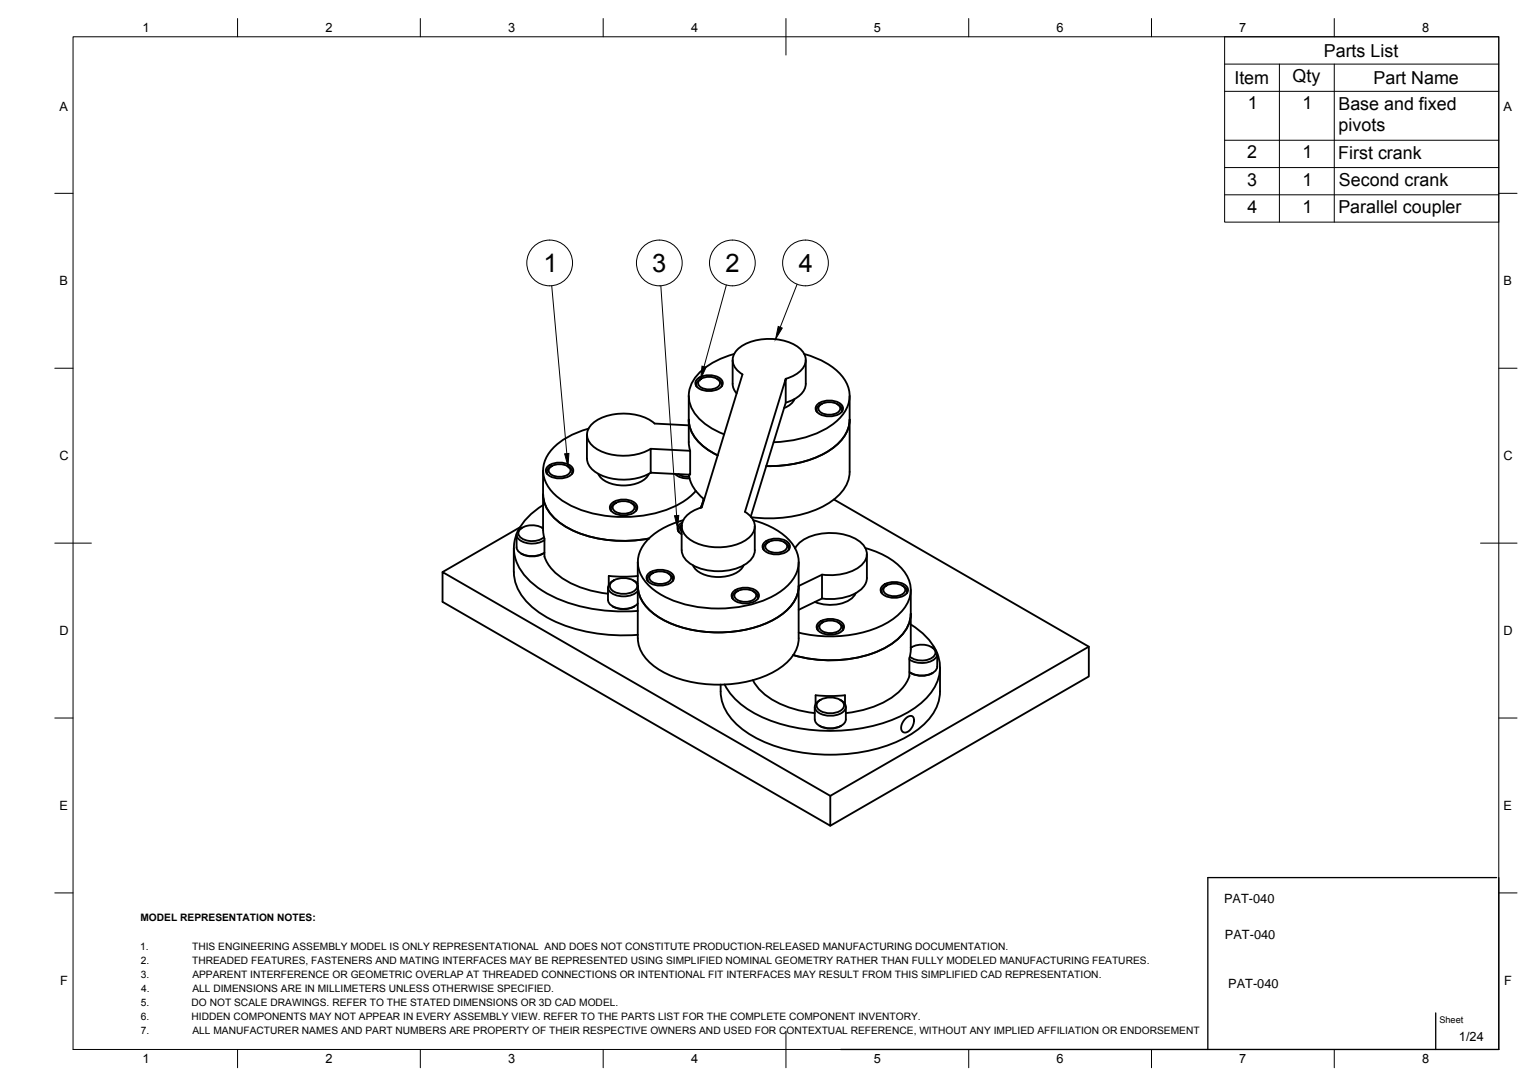
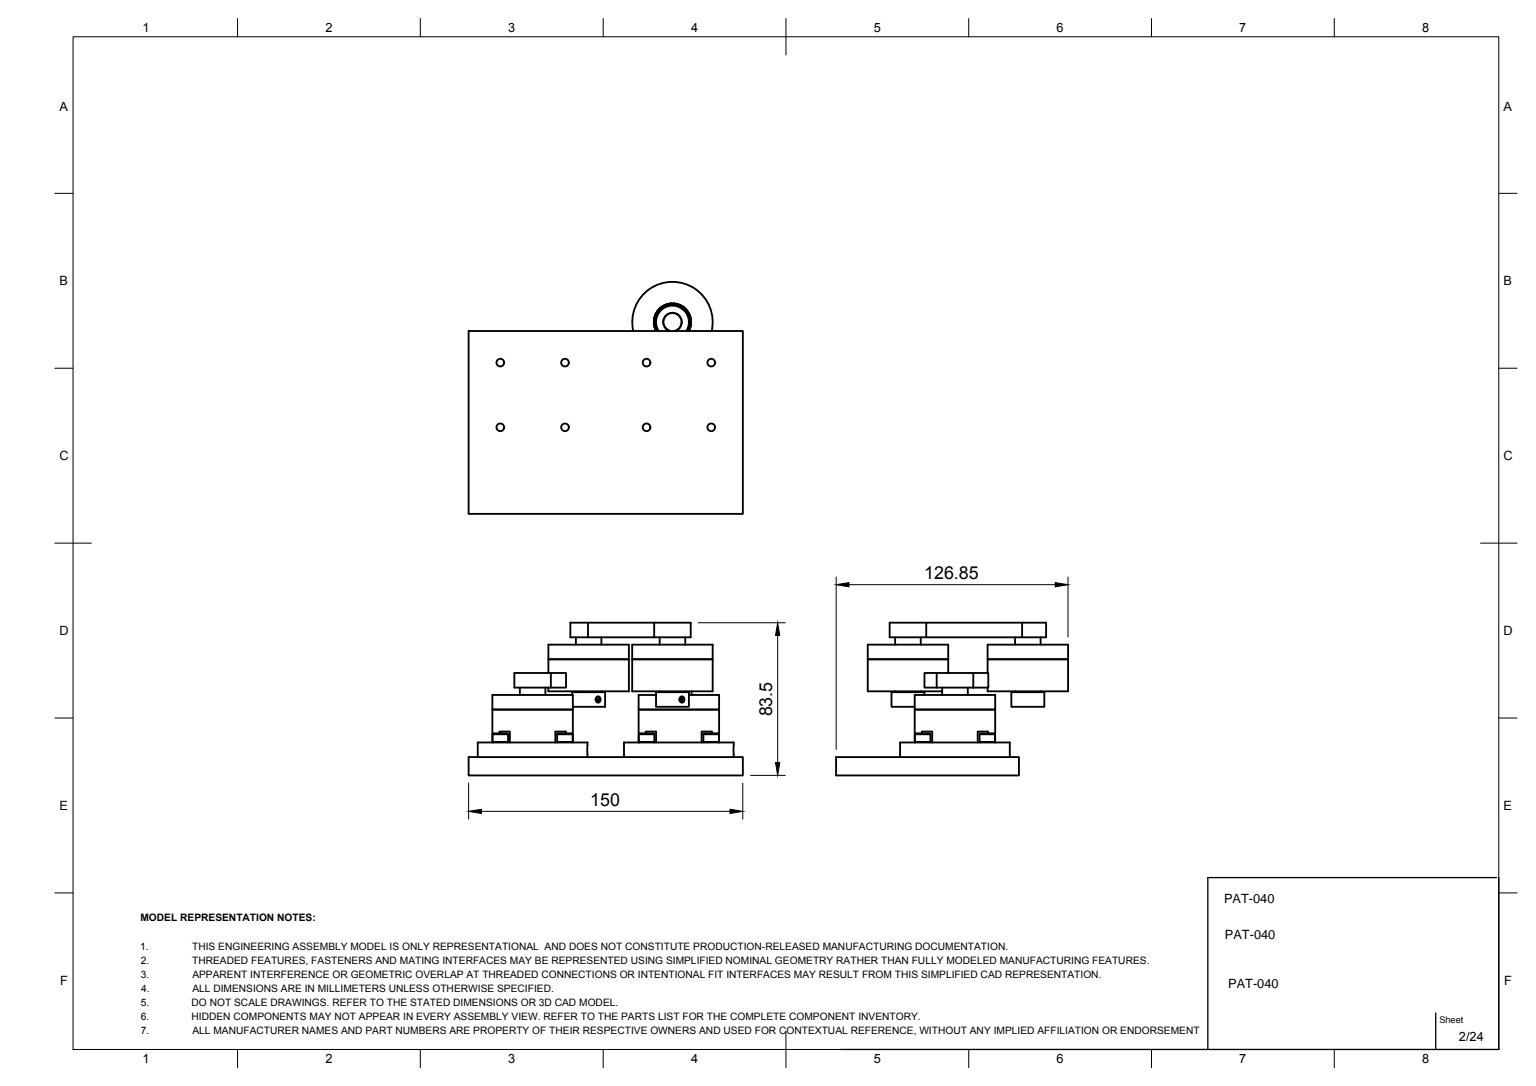
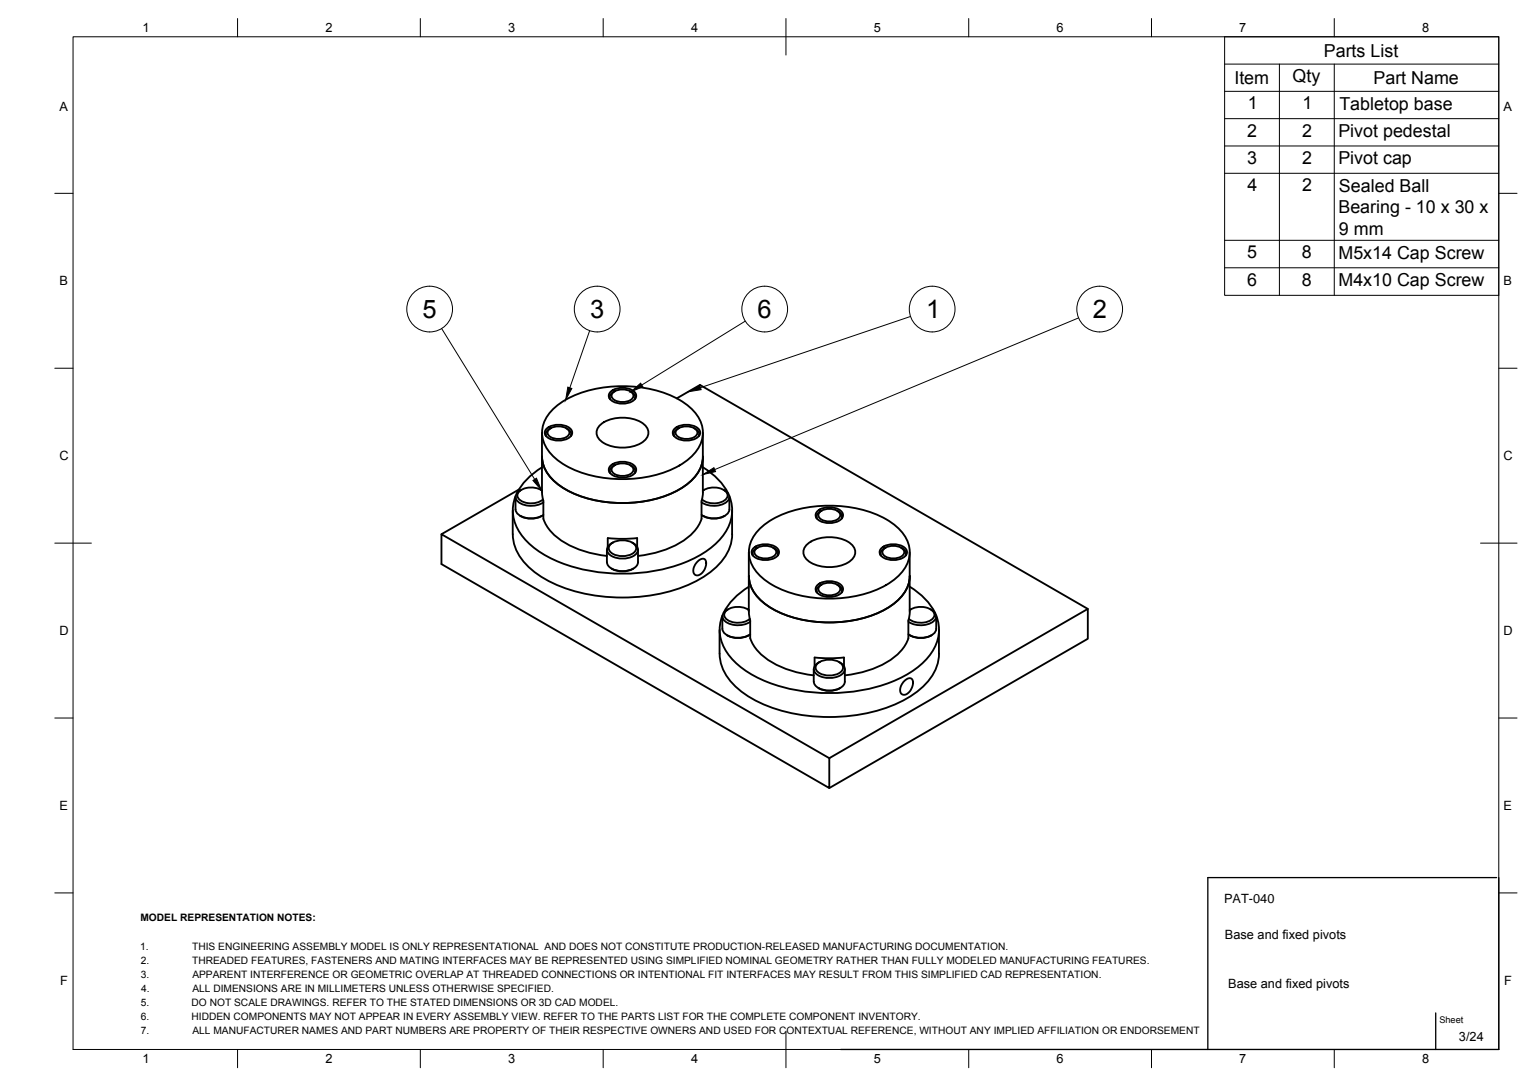
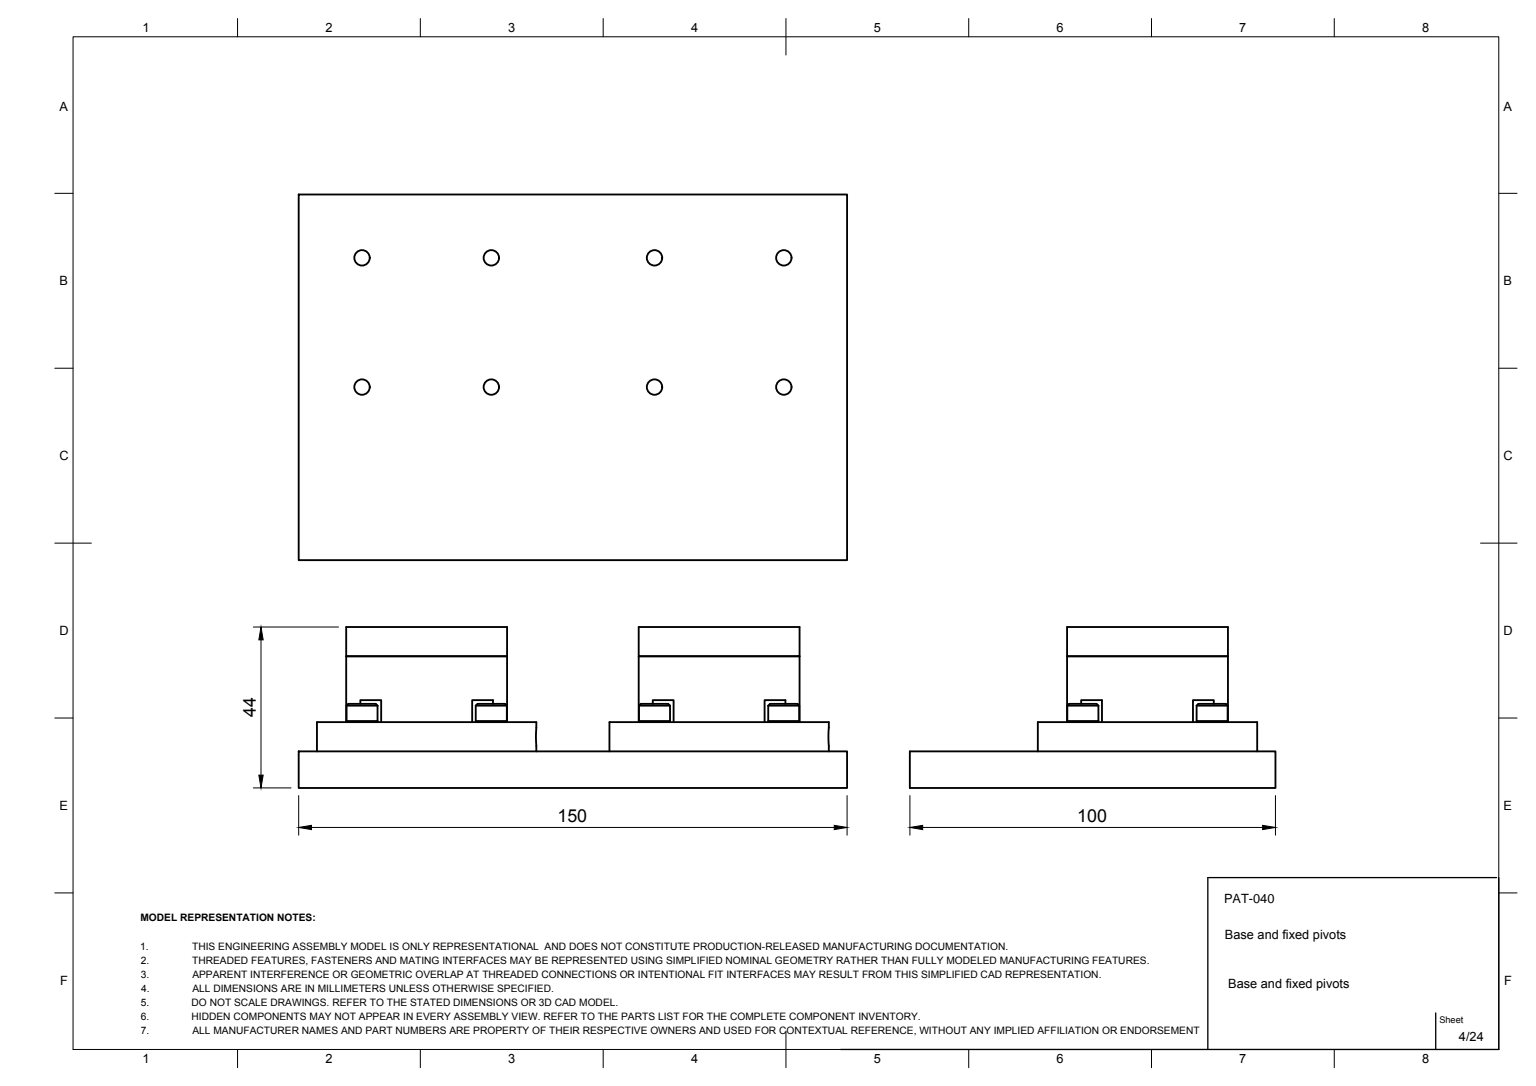
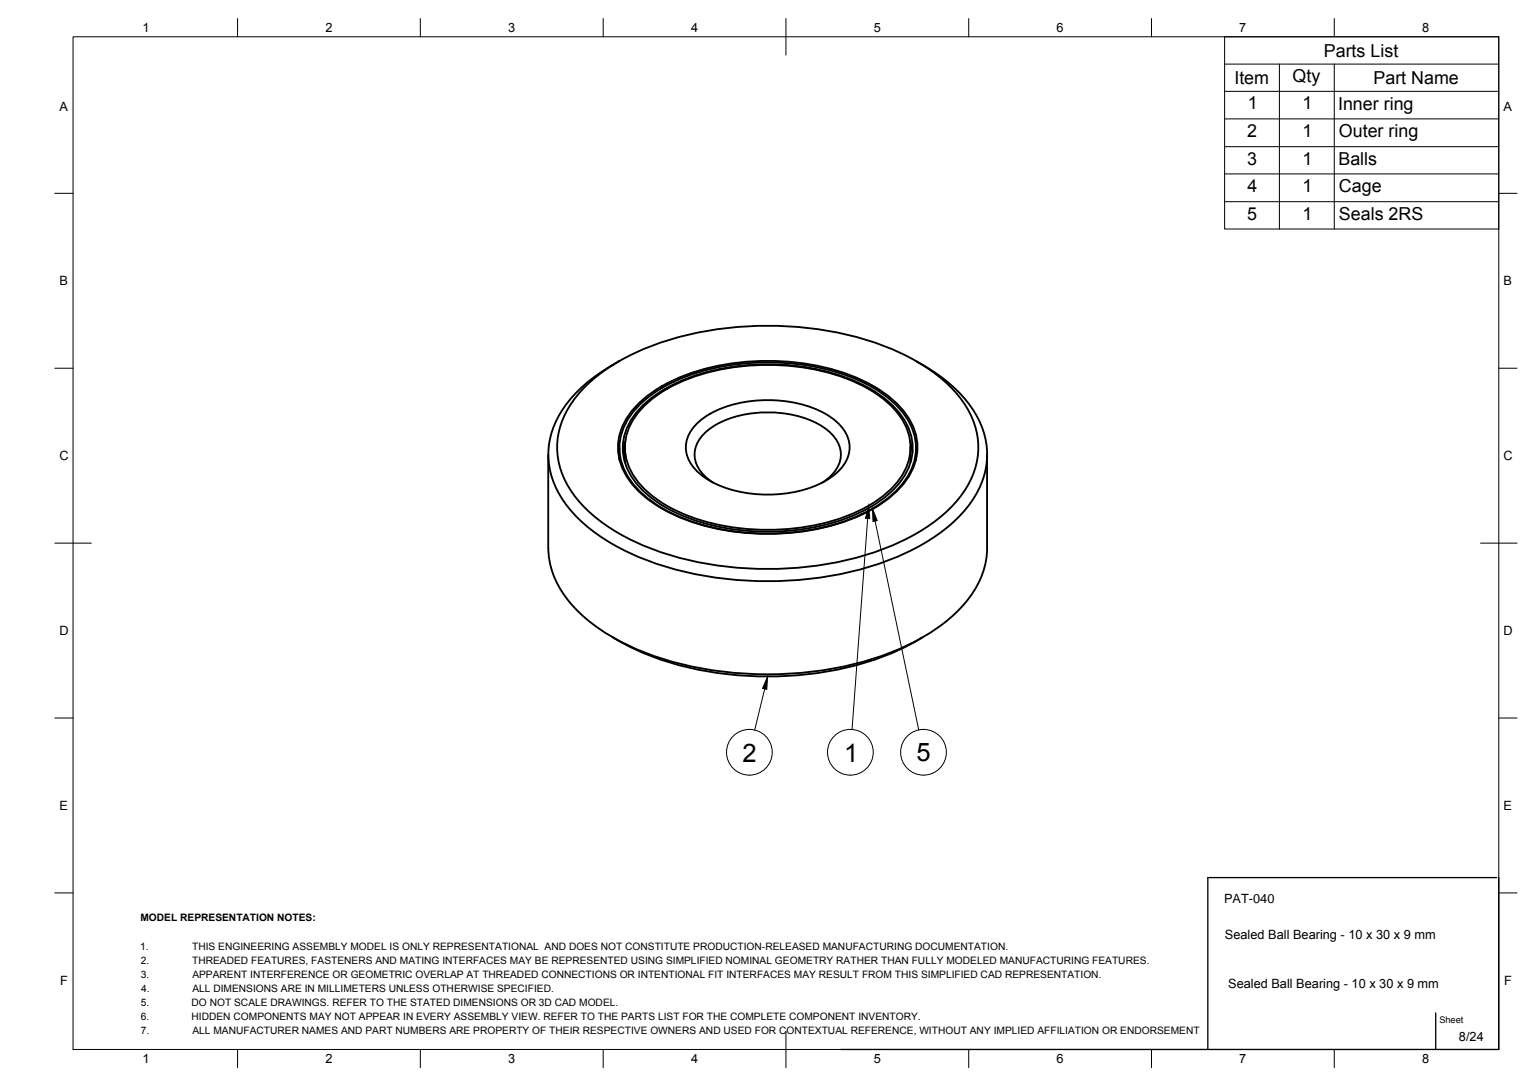
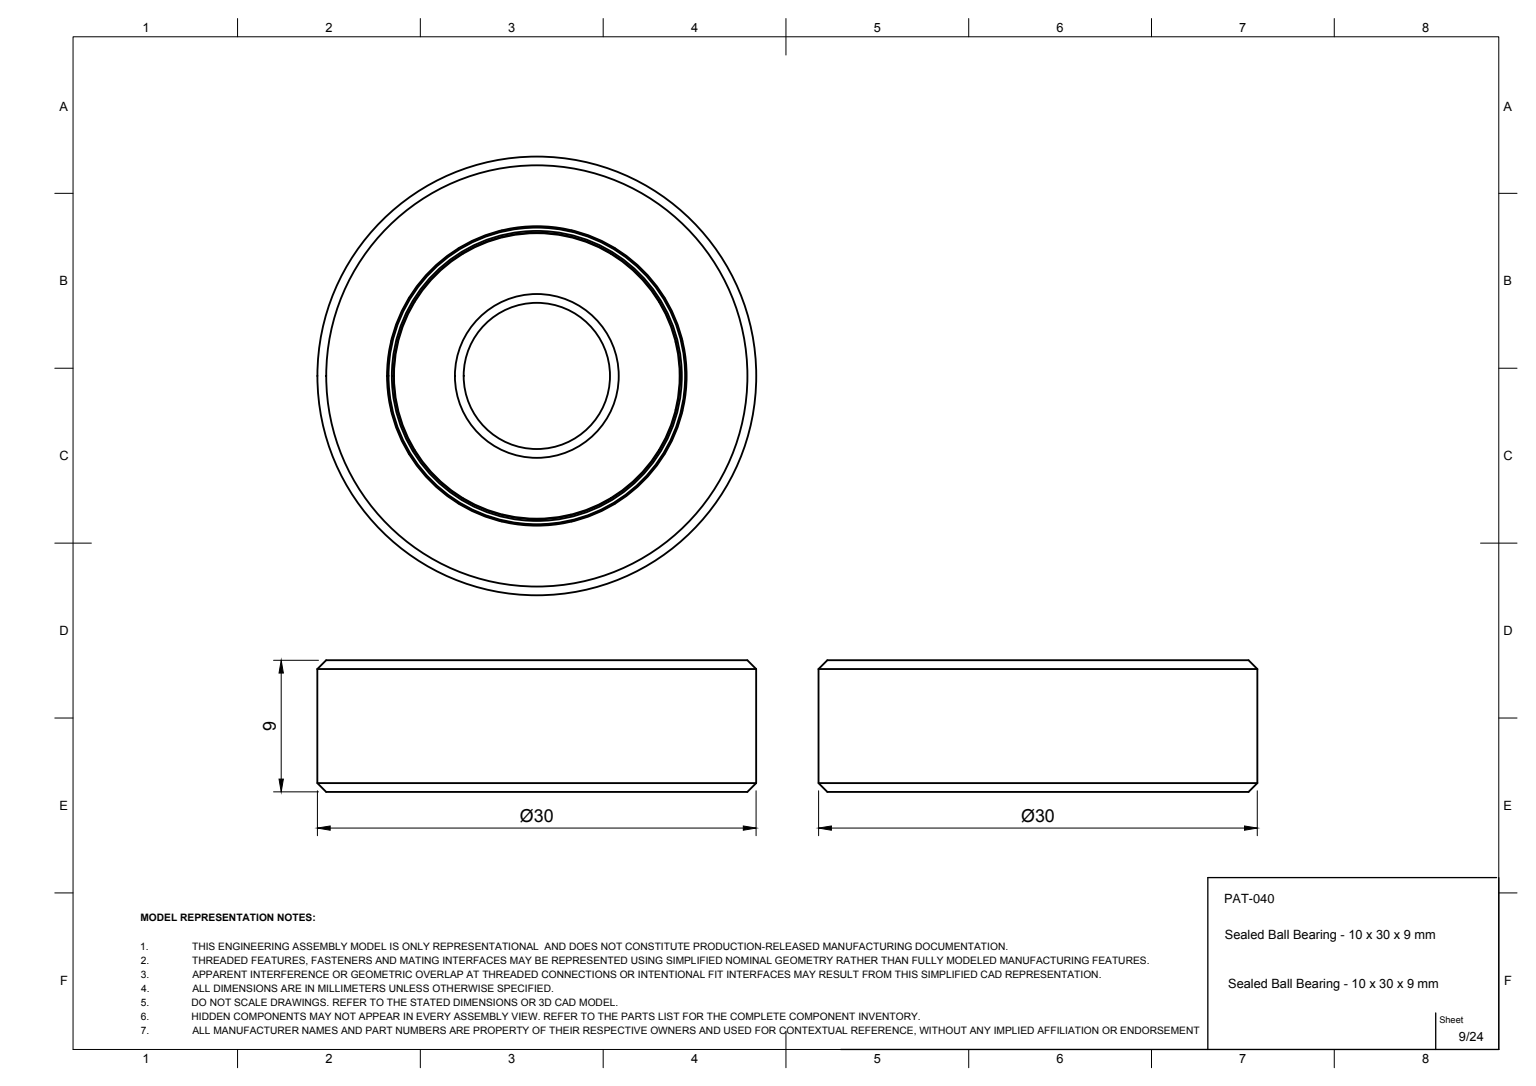
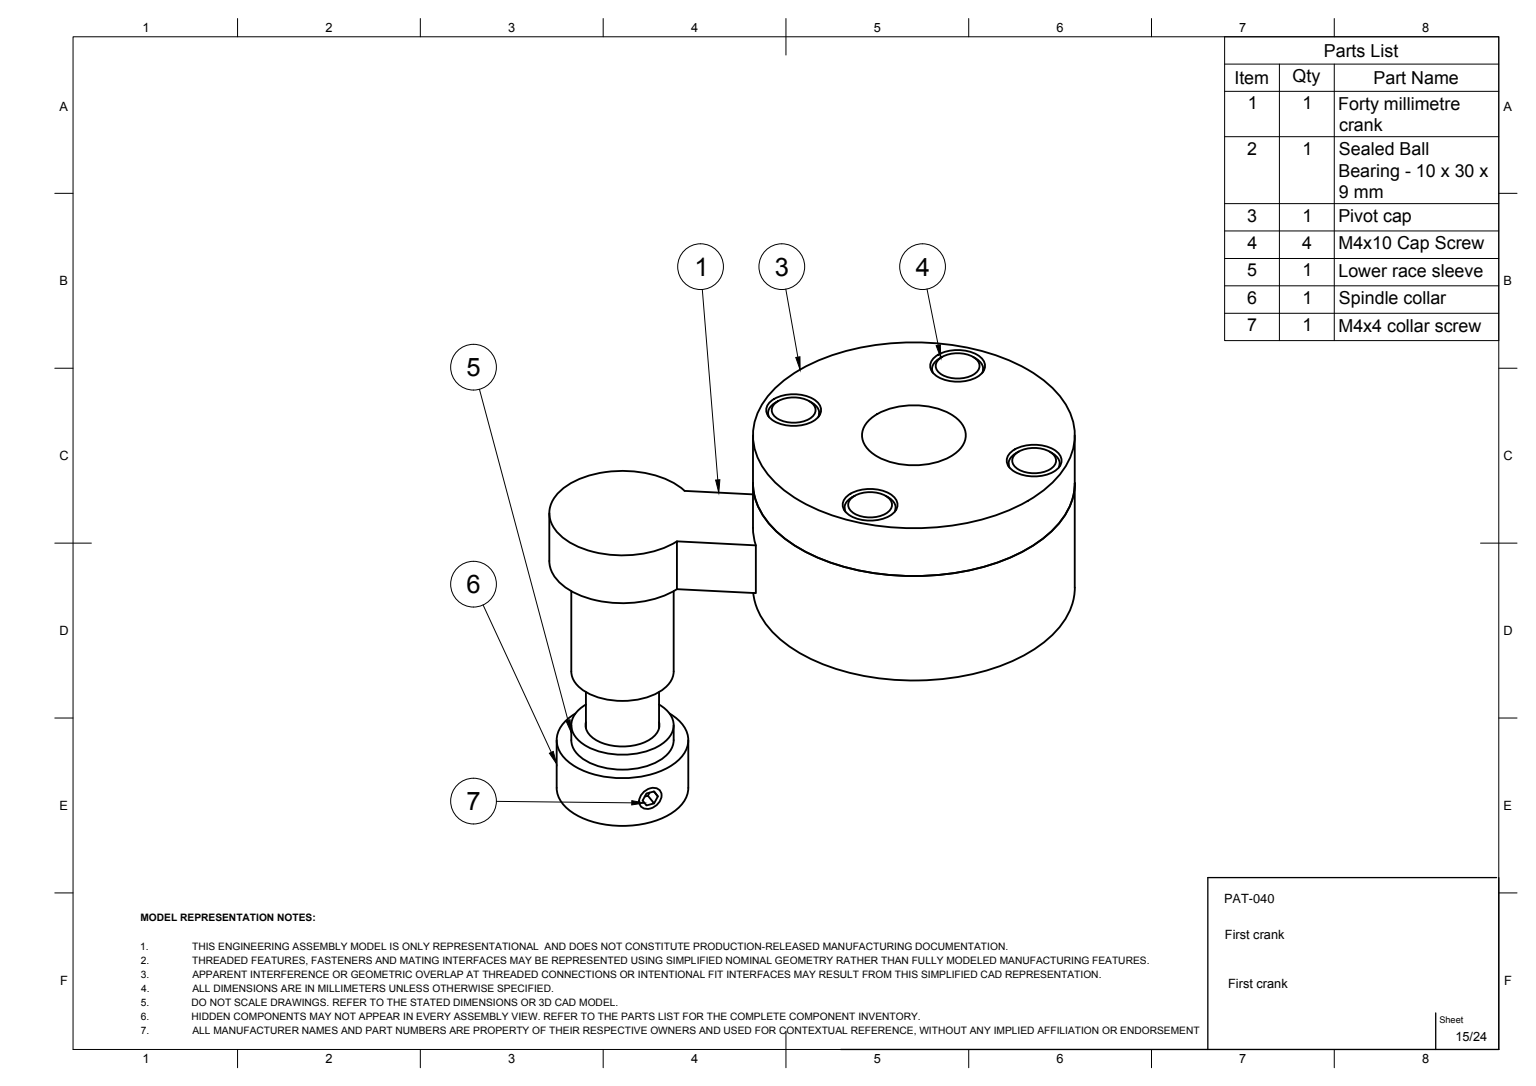
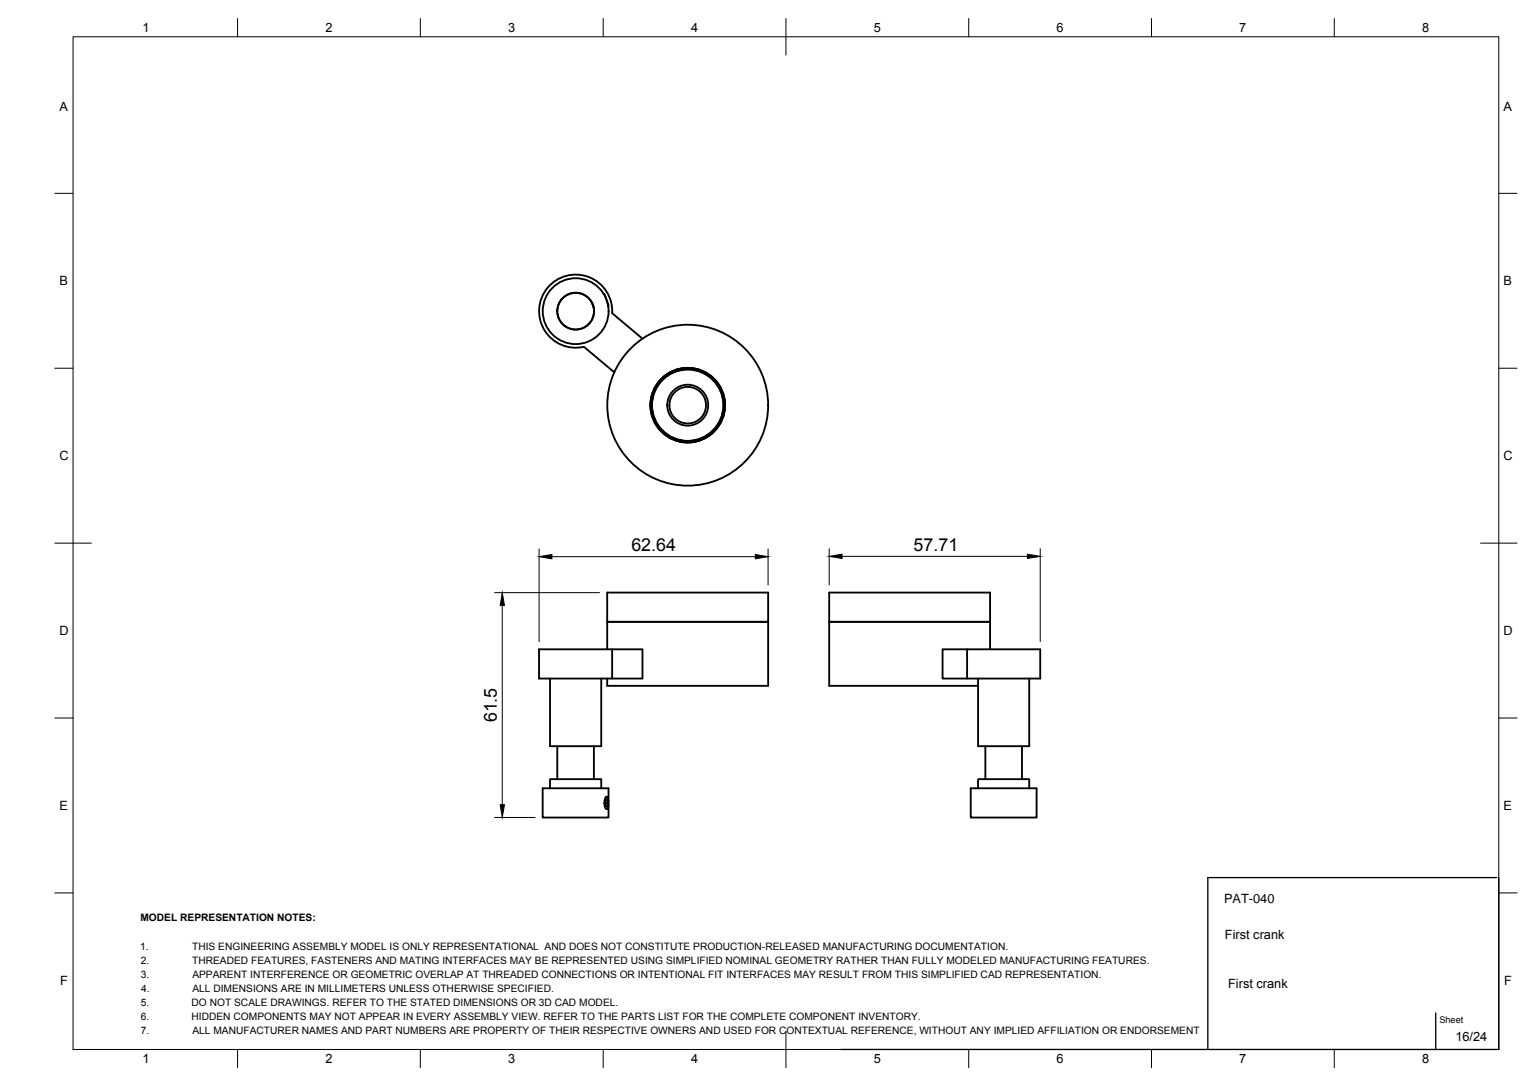
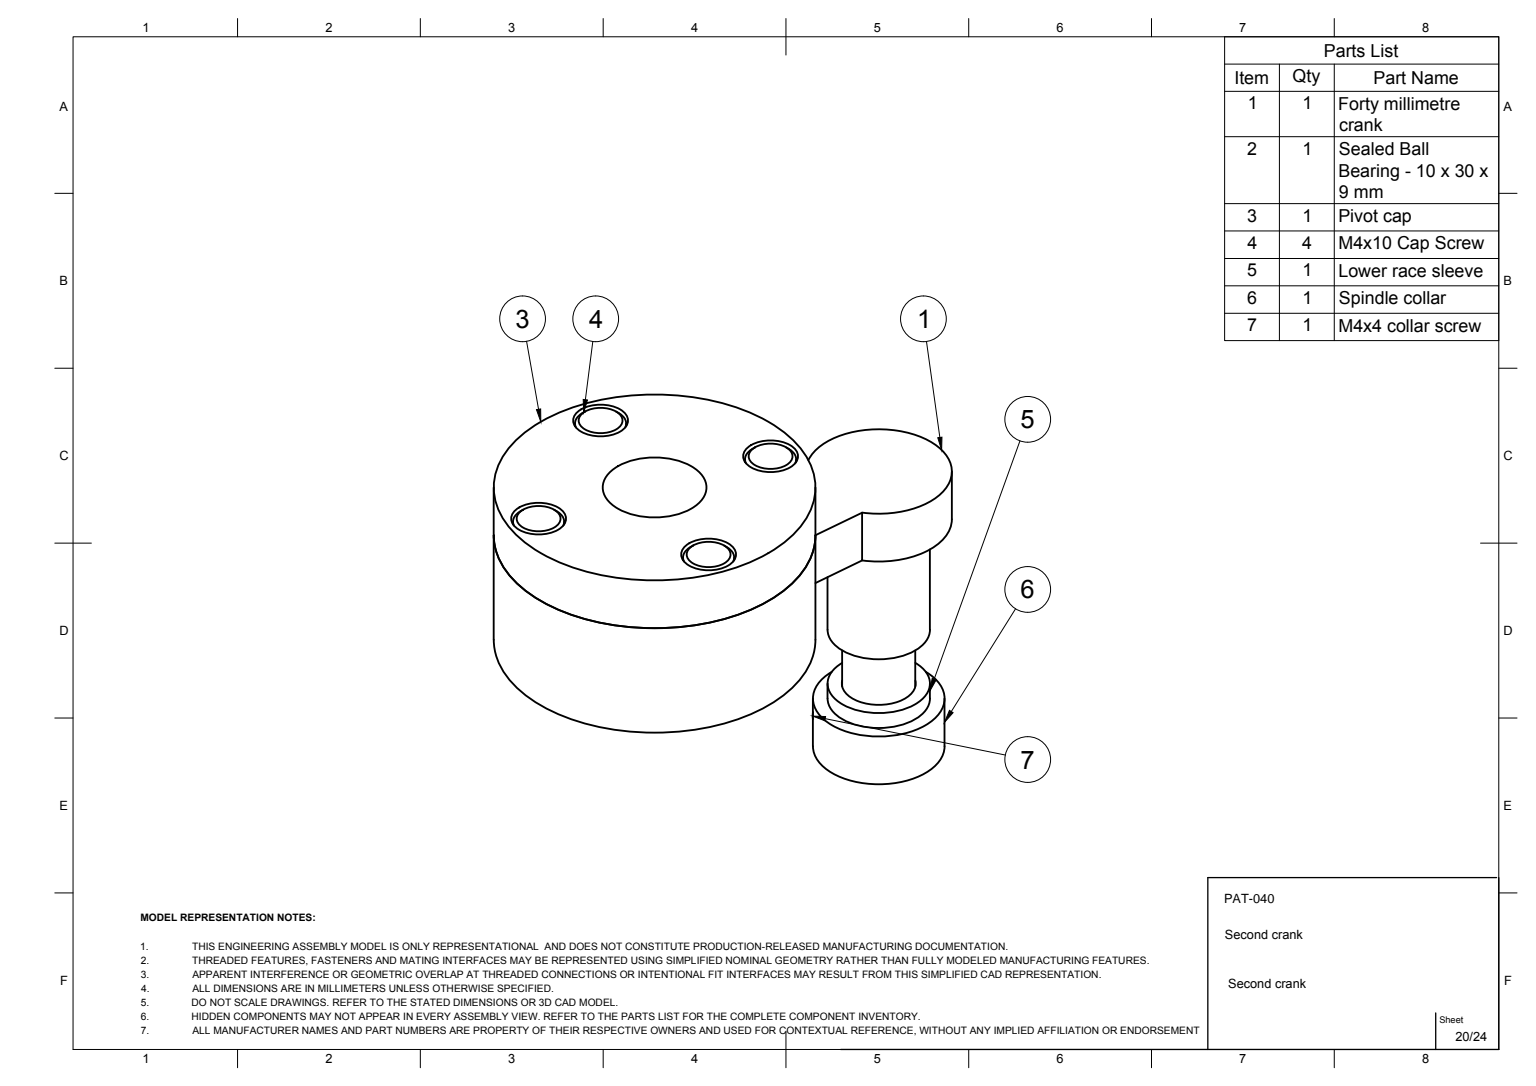
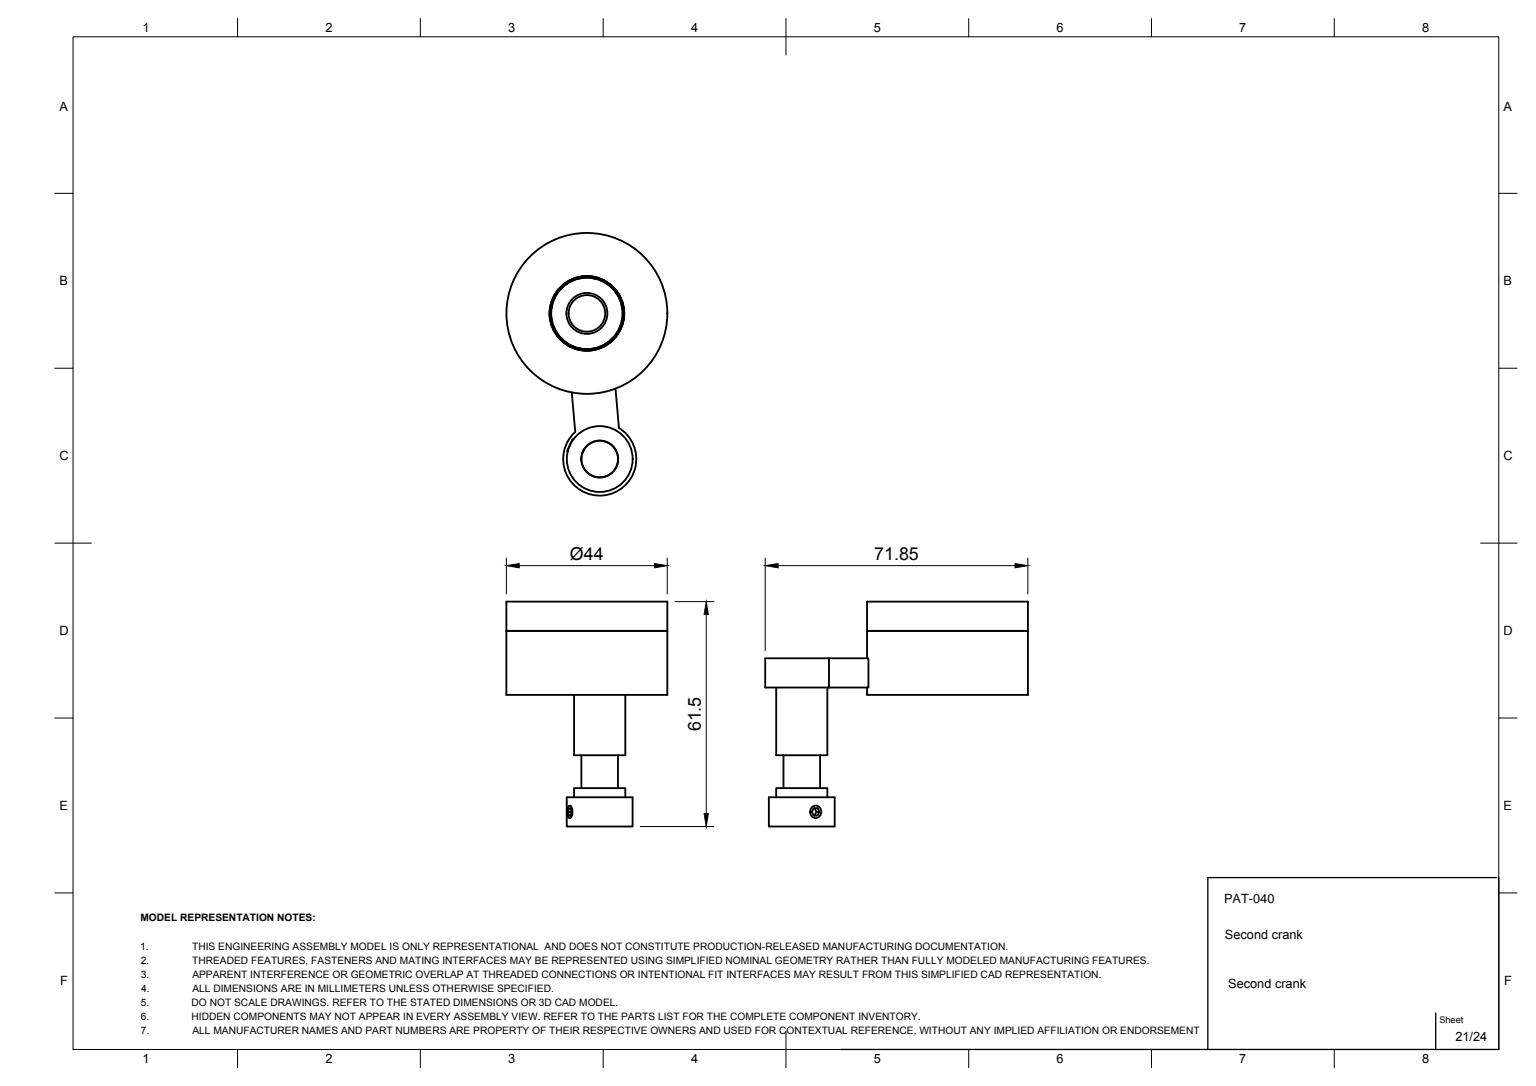
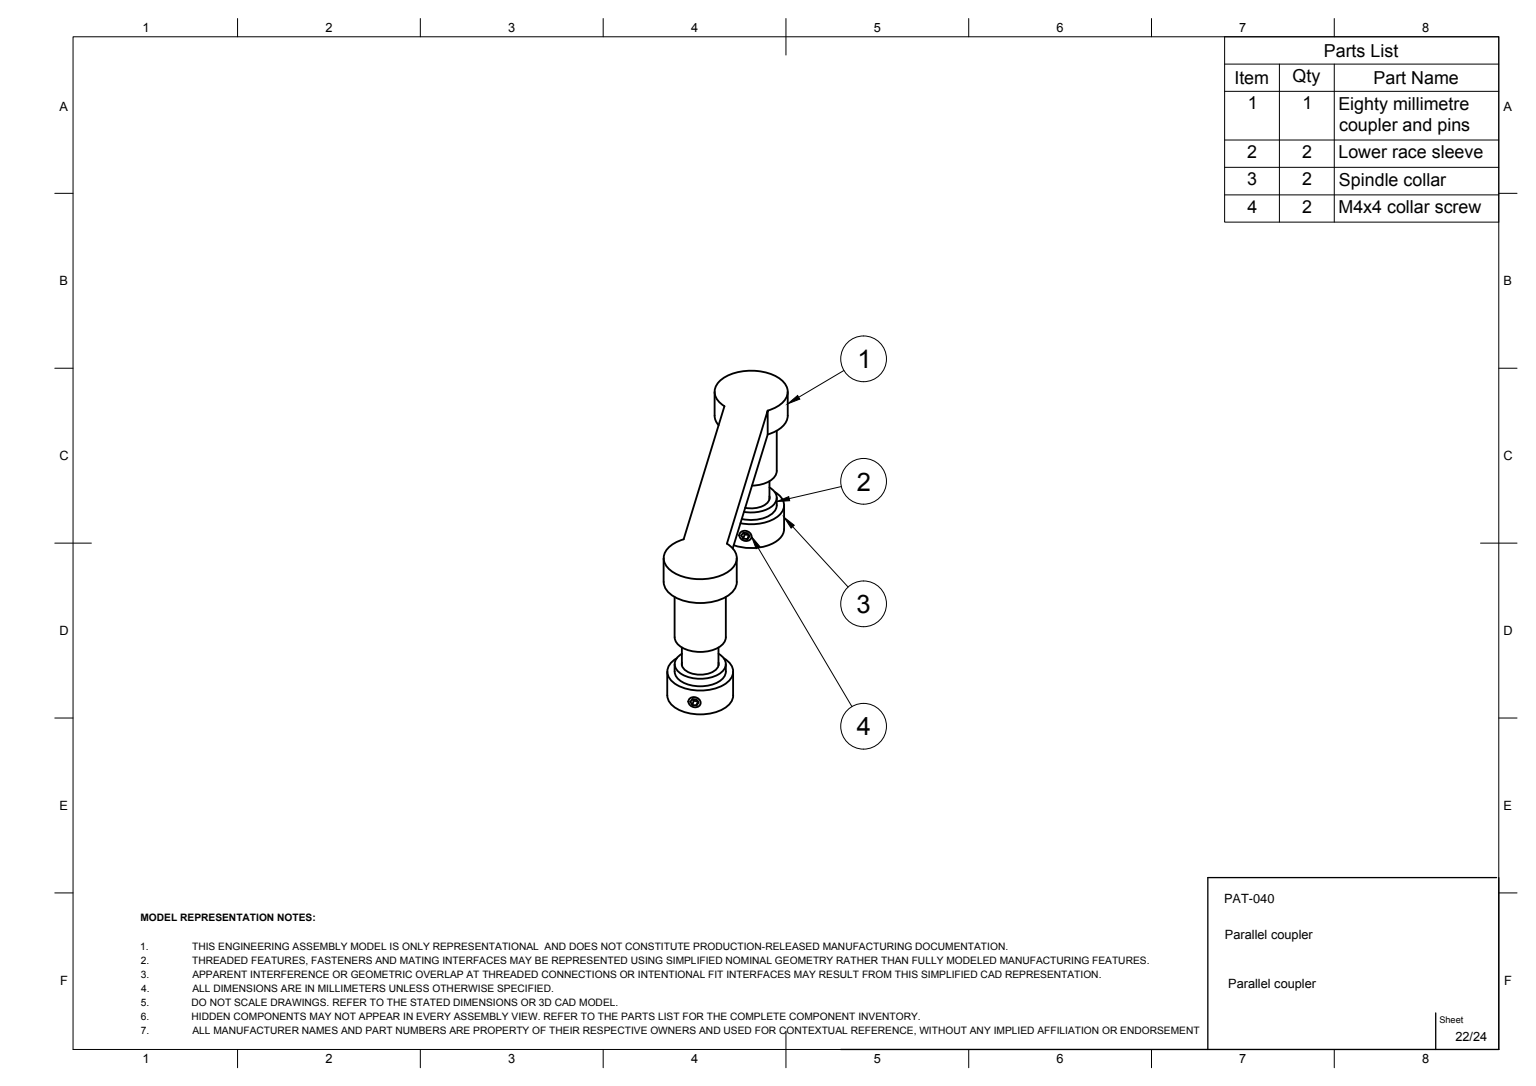
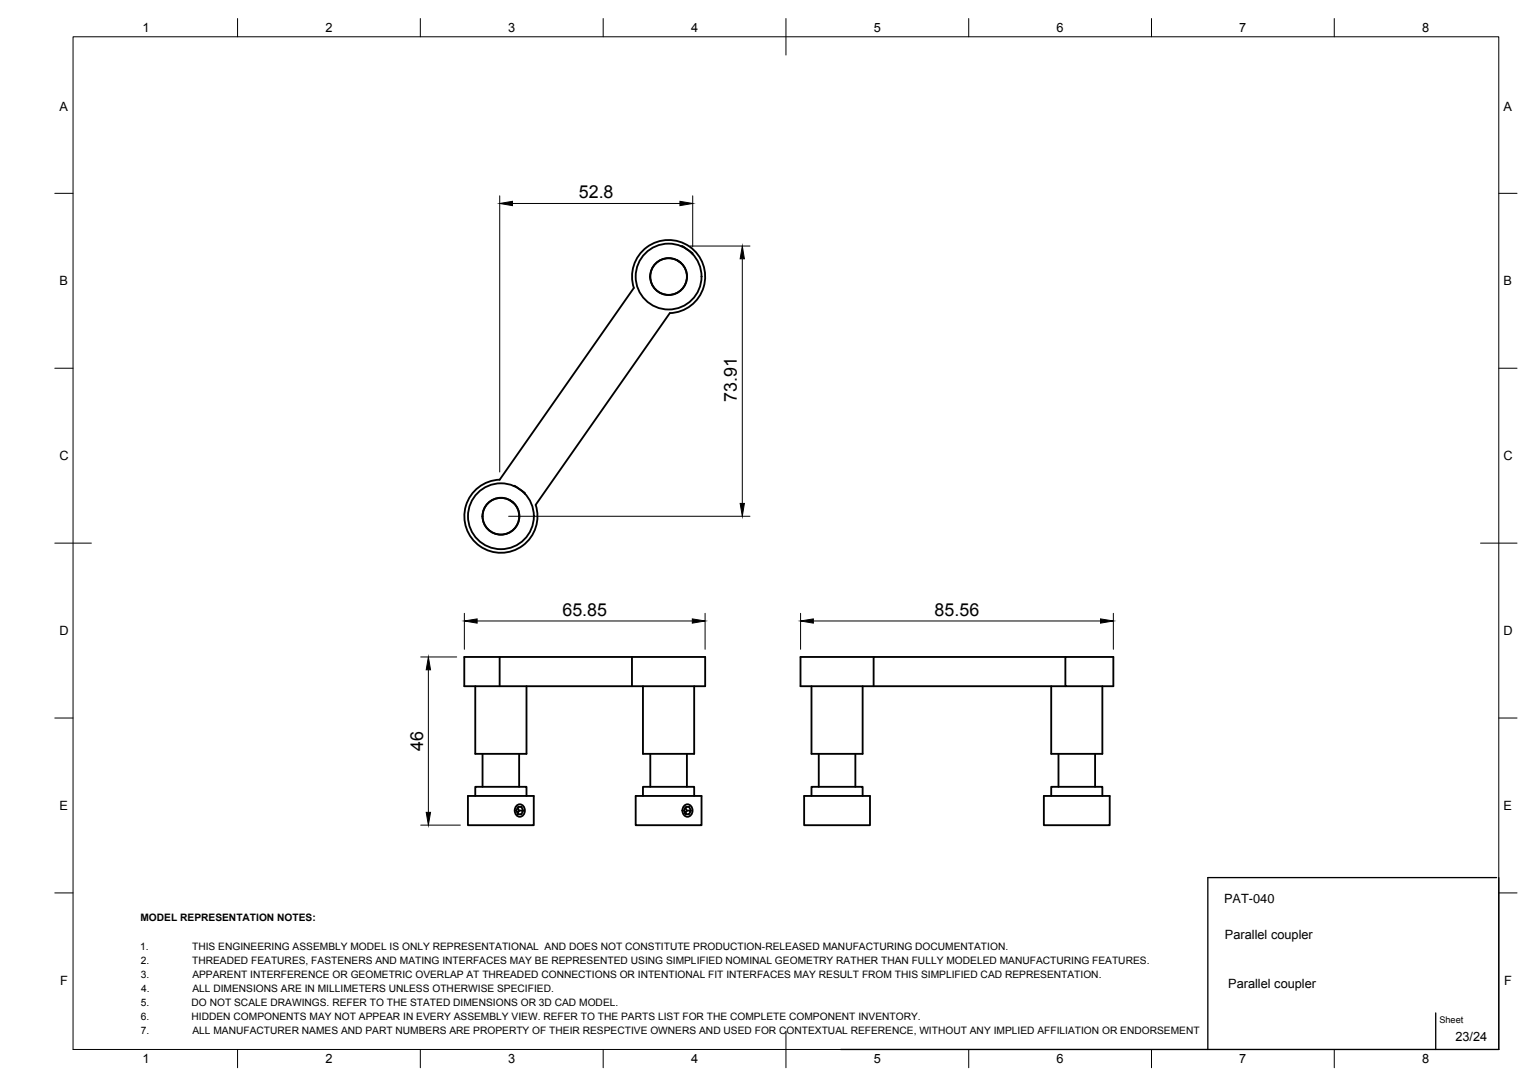
ISO-10303-21;
HEADER;
/* Generated by software containing ST-Developer
 * from STEP Tools, Inc. (www.steptools.com) 
 */

FILE_DESCRIPTION(
/* description */ ('Four-bar tabletop demonstrator'),
/* implementation_level */ '2;1');

FILE_NAME(
/* name */ 'PAT-040',
/* time_stamp */ '2026-10-29T17:05:23-07:00',
/* author */ (''),
/* organization */ (''),
/* preprocessor_version */ 'ST-DEVELOPER v20.2',
/* originating_system */ 'Autodesk Translation Framework v15.17.0.0',
/* authorisation */ '');

FILE_SCHEMA (('AUTOMOTIVE_DESIGN { 1 0 10303 214 3 1 1 }'));
ENDSEC;

DATA;
#10=MECHANICAL_DESIGN_GEOMETRIC_PRESENTATION_REPRESENTATION('',(#337,#338,
#339,#340,#341,#342,#343,#344,#345,#346,#347,#348,#349,#350,#351,#352,#353,
#354,#355,#356,#357,#358,#359),#6705);
#11=ITEM_DEFINED_TRANSFORMATION($,$,#3748,#3876);
#12=ITEM_DEFINED_TRANSFORMATION($,$,#3768,#3877);
#13=ITEM_DEFINED_TRANSFORMATION($,$,#3788,#3878);
#14=ITEM_DEFINED_TRANSFORMATION($,$,#3805,#3879);
#15=ITEM_DEFINED_TRANSFORMATION($,$,#3859,#3880);
#16=ITEM_DEFINED_TRANSFORMATION($,$,#3574,#3946);
#17=ITEM_DEFINED_TRANSFORMATION($,$,#3605,#3947);
#18=ITEM_DEFINED_TRANSFORMATION($,$,#3881,#3948);
#19=ITEM_DEFINED_TRANSFORMATION($,$,#3747,#3949);
#20=ITEM_DEFINED_TRANSFORMATION($,$,#3675,#3950);
#21=ITEM_DEFINED_TRANSFORMATION($,$,#3675,#3951);
#22=ITEM_DEFINED_TRANSFORMATION($,$,#3675,#3952);
#23=ITEM_DEFINED_TRANSFORMATION($,$,#3675,#3953);
#24=ITEM_DEFINED_TRANSFORMATION($,$,#3922,#3954);
#25=ITEM_DEFINED_TRANSFORMATION($,$,#3922,#3955);
#26=ITEM_DEFINED_TRANSFORMATION($,$,#3922,#3956);
#27=ITEM_DEFINED_TRANSFORMATION($,$,#3922,#3957);
#28=ITEM_DEFINED_TRANSFORMATION($,$,#3605,#3958);
#29=ITEM_DEFINED_TRANSFORMATION($,$,#3881,#3959);
#30=ITEM_DEFINED_TRANSFORMATION($,$,#3747,#3960);
#31=ITEM_DEFINED_TRANSFORMATION($,$,#3675,#3961);
#32=ITEM_DEFINED_TRANSFORMATION($,$,#3675,#3962);
#33=ITEM_DEFINED_TRANSFORMATION($,$,#3675,#3963);
#34=ITEM_DEFINED_TRANSFORMATION($,$,#3675,#3964);
#35=ITEM_DEFINED_TRANSFORMATION($,$,#3922,#3965);
#36=ITEM_DEFINED_TRANSFORMATION($,$,#3922,#3966);
#37=ITEM_DEFINED_TRANSFORMATION($,$,#3922,#3967);
#38=ITEM_DEFINED_TRANSFORMATION($,$,#3922,#3968);
#39=ITEM_DEFINED_TRANSFORMATION($,$,#3701,#4035);
#40=ITEM_DEFINED_TRANSFORMATION($,$,#3747,#4036);
#41=ITEM_DEFINED_TRANSFORMATION($,$,#3881,#4037);
#42=ITEM_DEFINED_TRANSFORMATION($,$,#3922,#4038);
#43=ITEM_DEFINED_TRANSFORMATION($,$,#3922,#4039);
#44=ITEM_DEFINED_TRANSFORMATION($,$,#3922,#4040);
#45=ITEM_DEFINED_TRANSFORMATION($,$,#3922,#4041);
#46=ITEM_DEFINED_TRANSFORMATION($,$,#3997,#4042);
#47=ITEM_DEFINED_TRANSFORMATION($,$,#4006,#4043);
#48=ITEM_DEFINED_TRANSFORMATION($,$,#4020,#4044);
#49=ITEM_DEFINED_TRANSFORMATION($,$,#3701,#4045);
#50=ITEM_DEFINED_TRANSFORMATION($,$,#3747,#4046);
#51=ITEM_DEFINED_TRANSFORMATION($,$,#3881,#4047);
#52=ITEM_DEFINED_TRANSFORMATION($,$,#3922,#4048);
#53=ITEM_DEFINED_TRANSFORMATION($,$,#3922,#4049);
#54=ITEM_DEFINED_TRANSFORMATION($,$,#3922,#4050);
#55=ITEM_DEFINED_TRANSFORMATION($,$,#3922,#4051);
#56=ITEM_DEFINED_TRANSFORMATION($,$,#3997,#4052);
#57=ITEM_DEFINED_TRANSFORMATION($,$,#4006,#4053);
#58=ITEM_DEFINED_TRANSFORMATION($,$,#4020,#4054);
#59=ITEM_DEFINED_TRANSFORMATION($,$,#3970,#4055);
#60=ITEM_DEFINED_TRANSFORMATION($,$,#3997,#4056);
#61=ITEM_DEFINED_TRANSFORMATION($,$,#4006,#4057);
#62=ITEM_DEFINED_TRANSFORMATION($,$,#4020,#4058);
#63=ITEM_DEFINED_TRANSFORMATION($,$,#3997,#4059);
#64=ITEM_DEFINED_TRANSFORMATION($,$,#4006,#4060);
#65=ITEM_DEFINED_TRANSFORMATION($,$,#4020,#4061);
#66=ITEM_DEFINED_TRANSFORMATION($,$,#3573,#4062);
#67=ITEM_DEFINED_TRANSFORMATION($,$,#3699,#4063);
#68=ITEM_DEFINED_TRANSFORMATION($,$,#3700,#4064);
#69=ITEM_DEFINED_TRANSFORMATION($,$,#3969,#4065);
#70=(
REPRESENTATION_RELATIONSHIP($,$,#6820,#6819)
REPRESENTATION_RELATIONSHIP_WITH_TRANSFORMATION(#11)
SHAPE_REPRESENTATION_RELATIONSHIP()
);
#71=(
REPRESENTATION_RELATIONSHIP($,$,#6821,#6819)
REPRESENTATION_RELATIONSHIP_WITH_TRANSFORMATION(#12)
SHAPE_REPRESENTATION_RELATIONSHIP()
);
#72=(
REPRESENTATION_RELATIONSHIP($,$,#6822,#6819)
REPRESENTATION_RELATIONSHIP_WITH_TRANSFORMATION(#13)
SHAPE_REPRESENTATION_RELATIONSHIP()
);
#73=(
REPRESENTATION_RELATIONSHIP($,$,#6823,#6819)
REPRESENTATION_RELATIONSHIP_WITH_TRANSFORMATION(#14)
SHAPE_REPRESENTATION_RELATIONSHIP()
);
#74=(
REPRESENTATION_RELATIONSHIP($,$,#6824,#6819)
REPRESENTATION_RELATIONSHIP_WITH_TRANSFORMATION(#15)
SHAPE_REPRESENTATION_RELATIONSHIP()
);
#75=(
REPRESENTATION_RELATIONSHIP($,$,#6813,#6812)
REPRESENTATION_RELATIONSHIP_WITH_TRANSFORMATION(#16)
SHAPE_REPRESENTATION_RELATIONSHIP()
);
#76=(
REPRESENTATION_RELATIONSHIP($,$,#6814,#6812)
REPRESENTATION_RELATIONSHIP_WITH_TRANSFORMATION(#17)
SHAPE_REPRESENTATION_RELATIONSHIP()
);
#77=(
REPRESENTATION_RELATIONSHIP($,$,#6825,#6812)
REPRESENTATION_RELATIONSHIP_WITH_TRANSFORMATION(#18)
SHAPE_REPRESENTATION_RELATIONSHIP()
);
#78=(
REPRESENTATION_RELATIONSHIP($,$,#6819,#6812)
REPRESENTATION_RELATIONSHIP_WITH_TRANSFORMATION(#19)
SHAPE_REPRESENTATION_RELATIONSHIP()
);
#79=(
REPRESENTATION_RELATIONSHIP($,$,#6815,#6812)
REPRESENTATION_RELATIONSHIP_WITH_TRANSFORMATION(#20)
SHAPE_REPRESENTATION_RELATIONSHIP()
);
#80=(
REPRESENTATION_RELATIONSHIP($,$,#6815,#6812)
REPRESENTATION_RELATIONSHIP_WITH_TRANSFORMATION(#21)
SHAPE_REPRESENTATION_RELATIONSHIP()
);
#81=(
REPRESENTATION_RELATIONSHIP($,$,#6815,#6812)
REPRESENTATION_RELATIONSHIP_WITH_TRANSFORMATION(#22)
SHAPE_REPRESENTATION_RELATIONSHIP()
);
#82=(
REPRESENTATION_RELATIONSHIP($,$,#6815,#6812)
REPRESENTATION_RELATIONSHIP_WITH_TRANSFORMATION(#23)
SHAPE_REPRESENTATION_RELATIONSHIP()
);
#83=(
REPRESENTATION_RELATIONSHIP($,$,#6826,#6812)
REPRESENTATION_RELATIONSHIP_WITH_TRANSFORMATION(#24)
SHAPE_REPRESENTATION_RELATIONSHIP()
);
#84=(
REPRESENTATION_RELATIONSHIP($,$,#6826,#6812)
REPRESENTATION_RELATIONSHIP_WITH_TRANSFORMATION(#25)
SHAPE_REPRESENTATION_RELATIONSHIP()
);
#85=(
REPRESENTATION_RELATIONSHIP($,$,#6826,#6812)
REPRESENTATION_RELATIONSHIP_WITH_TRANSFORMATION(#26)
SHAPE_REPRESENTATION_RELATIONSHIP()
);
#86=(
REPRESENTATION_RELATIONSHIP($,$,#6826,#6812)
REPRESENTATION_RELATIONSHIP_WITH_TRANSFORMATION(#27)
SHAPE_REPRESENTATION_RELATIONSHIP()
);
#87=(
REPRESENTATION_RELATIONSHIP($,$,#6814,#6812)
REPRESENTATION_RELATIONSHIP_WITH_TRANSFORMATION(#28)
SHAPE_REPRESENTATION_RELATIONSHIP()
);
#88=(
REPRESENTATION_RELATIONSHIP($,$,#6825,#6812)
REPRESENTATION_RELATIONSHIP_WITH_TRANSFORMATION(#29)
SHAPE_REPRESENTATION_RELATIONSHIP()
);
#89=(
REPRESENTATION_RELATIONSHIP($,$,#6819,#6812)
REPRESENTATION_RELATIONSHIP_WITH_TRANSFORMATION(#30)
SHAPE_REPRESENTATION_RELATIONSHIP()
);
#90=(
REPRESENTATION_RELATIONSHIP($,$,#6815,#6812)
REPRESENTATION_RELATIONSHIP_WITH_TRANSFORMATION(#31)
SHAPE_REPRESENTATION_RELATIONSHIP()
);
#91=(
REPRESENTATION_RELATIONSHIP($,$,#6815,#6812)
REPRESENTATION_RELATIONSHIP_WITH_TRANSFORMATION(#32)
SHAPE_REPRESENTATION_RELATIONSHIP()
);
#92=(
REPRESENTATION_RELATIONSHIP($,$,#6815,#6812)
REPRESENTATION_RELATIONSHIP_WITH_TRANSFORMATION(#33)
SHAPE_REPRESENTATION_RELATIONSHIP()
);
#93=(
REPRESENTATION_RELATIONSHIP($,$,#6815,#6812)
REPRESENTATION_RELATIONSHIP_WITH_TRANSFORMATION(#34)
SHAPE_REPRESENTATION_RELATIONSHIP()
);
#94=(
REPRESENTATION_RELATIONSHIP($,$,#6826,#6812)
REPRESENTATION_RELATIONSHIP_WITH_TRANSFORMATION(#35)
SHAPE_REPRESENTATION_RELATIONSHIP()
);
#95=(
REPRESENTATION_RELATIONSHIP($,$,#6826,#6812)
REPRESENTATION_RELATIONSHIP_WITH_TRANSFORMATION(#36)
SHAPE_REPRESENTATION_RELATIONSHIP()
);
#96=(
REPRESENTATION_RELATIONSHIP($,$,#6826,#6812)
REPRESENTATION_RELATIONSHIP_WITH_TRANSFORMATION(#37)
SHAPE_REPRESENTATION_RELATIONSHIP()
);
#97=(
REPRESENTATION_RELATIONSHIP($,$,#6826,#6812)
REPRESENTATION_RELATIONSHIP_WITH_TRANSFORMATION(#38)
SHAPE_REPRESENTATION_RELATIONSHIP()
);
#98=(
REPRESENTATION_RELATIONSHIP($,$,#6818,#6816)
REPRESENTATION_RELATIONSHIP_WITH_TRANSFORMATION(#39)
SHAPE_REPRESENTATION_RELATIONSHIP()
);
#99=(
REPRESENTATION_RELATIONSHIP($,$,#6819,#6816)
REPRESENTATION_RELATIONSHIP_WITH_TRANSFORMATION(#40)
SHAPE_REPRESENTATION_RELATIONSHIP()
);
#100=(
REPRESENTATION_RELATIONSHIP($,$,#6825,#6816)
REPRESENTATION_RELATIONSHIP_WITH_TRANSFORMATION(#41)
SHAPE_REPRESENTATION_RELATIONSHIP()
);
#101=(
REPRESENTATION_RELATIONSHIP($,$,#6826,#6816)
REPRESENTATION_RELATIONSHIP_WITH_TRANSFORMATION(#42)
SHAPE_REPRESENTATION_RELATIONSHIP()
);
#102=(
REPRESENTATION_RELATIONSHIP($,$,#6826,#6816)
REPRESENTATION_RELATIONSHIP_WITH_TRANSFORMATION(#43)
SHAPE_REPRESENTATION_RELATIONSHIP()
);
#103=(
REPRESENTATION_RELATIONSHIP($,$,#6826,#6816)
REPRESENTATION_RELATIONSHIP_WITH_TRANSFORMATION(#44)
SHAPE_REPRESENTATION_RELATIONSHIP()
);
#104=(
REPRESENTATION_RELATIONSHIP($,$,#6826,#6816)
REPRESENTATION_RELATIONSHIP_WITH_TRANSFORMATION(#45)
SHAPE_REPRESENTATION_RELATIONSHIP()
);
#105=(
REPRESENTATION_RELATIONSHIP($,$,#6829,#6816)
REPRESENTATION_RELATIONSHIP_WITH_TRANSFORMATION(#46)
SHAPE_REPRESENTATION_RELATIONSHIP()
);
#106=(
REPRESENTATION_RELATIONSHIP($,$,#6830,#6816)
REPRESENTATION_RELATIONSHIP_WITH_TRANSFORMATION(#47)
SHAPE_REPRESENTATION_RELATIONSHIP()
);
#107=(
REPRESENTATION_RELATIONSHIP($,$,#6831,#6816)
REPRESENTATION_RELATIONSHIP_WITH_TRANSFORMATION(#48)
SHAPE_REPRESENTATION_RELATIONSHIP()
);
#108=(
REPRESENTATION_RELATIONSHIP($,$,#6818,#6817)
REPRESENTATION_RELATIONSHIP_WITH_TRANSFORMATION(#49)
SHAPE_REPRESENTATION_RELATIONSHIP()
);
#109=(
REPRESENTATION_RELATIONSHIP($,$,#6819,#6817)
REPRESENTATION_RELATIONSHIP_WITH_TRANSFORMATION(#50)
SHAPE_REPRESENTATION_RELATIONSHIP()
);
#110=(
REPRESENTATION_RELATIONSHIP($,$,#6825,#6817)
REPRESENTATION_RELATIONSHIP_WITH_TRANSFORMATION(#51)
SHAPE_REPRESENTATION_RELATIONSHIP()
);
#111=(
REPRESENTATION_RELATIONSHIP($,$,#6826,#6817)
REPRESENTATION_RELATIONSHIP_WITH_TRANSFORMATION(#52)
SHAPE_REPRESENTATION_RELATIONSHIP()
);
#112=(
REPRESENTATION_RELATIONSHIP($,$,#6826,#6817)
REPRESENTATION_RELATIONSHIP_WITH_TRANSFORMATION(#53)
SHAPE_REPRESENTATION_RELATIONSHIP()
);
#113=(
REPRESENTATION_RELATIONSHIP($,$,#6826,#6817)
REPRESENTATION_RELATIONSHIP_WITH_TRANSFORMATION(#54)
SHAPE_REPRESENTATION_RELATIONSHIP()
);
#114=(
REPRESENTATION_RELATIONSHIP($,$,#6826,#6817)
REPRESENTATION_RELATIONSHIP_WITH_TRANSFORMATION(#55)
SHAPE_REPRESENTATION_RELATIONSHIP()
);
#115=(
REPRESENTATION_RELATIONSHIP($,$,#6829,#6817)
REPRESENTATION_RELATIONSHIP_WITH_TRANSFORMATION(#56)
SHAPE_REPRESENTATION_RELATIONSHIP()
);
#116=(
REPRESENTATION_RELATIONSHIP($,$,#6830,#6817)
REPRESENTATION_RELATIONSHIP_WITH_TRANSFORMATION(#57)
SHAPE_REPRESENTATION_RELATIONSHIP()
);
#117=(
REPRESENTATION_RELATIONSHIP($,$,#6831,#6817)
REPRESENTATION_RELATIONSHIP_WITH_TRANSFORMATION(#58)
SHAPE_REPRESENTATION_RELATIONSHIP()
);
#118=(
REPRESENTATION_RELATIONSHIP($,$,#6828,#6827)
REPRESENTATION_RELATIONSHIP_WITH_TRANSFORMATION(#59)
SHAPE_REPRESENTATION_RELATIONSHIP()
);
#119=(
REPRESENTATION_RELATIONSHIP($,$,#6829,#6827)
REPRESENTATION_RELATIONSHIP_WITH_TRANSFORMATION(#60)
SHAPE_REPRESENTATION_RELATIONSHIP()
);
#120=(
REPRESENTATION_RELATIONSHIP($,$,#6830,#6827)
REPRESENTATION_RELATIONSHIP_WITH_TRANSFORMATION(#61)
SHAPE_REPRESENTATION_RELATIONSHIP()
);
#121=(
REPRESENTATION_RELATIONSHIP($,$,#6831,#6827)
REPRESENTATION_RELATIONSHIP_WITH_TRANSFORMATION(#62)
SHAPE_REPRESENTATION_RELATIONSHIP()
);
#122=(
REPRESENTATION_RELATIONSHIP($,$,#6829,#6827)
REPRESENTATION_RELATIONSHIP_WITH_TRANSFORMATION(#63)
SHAPE_REPRESENTATION_RELATIONSHIP()
);
#123=(
REPRESENTATION_RELATIONSHIP($,$,#6830,#6827)
REPRESENTATION_RELATIONSHIP_WITH_TRANSFORMATION(#64)
SHAPE_REPRESENTATION_RELATIONSHIP()
);
#124=(
REPRESENTATION_RELATIONSHIP($,$,#6831,#6827)
REPRESENTATION_RELATIONSHIP_WITH_TRANSFORMATION(#65)
SHAPE_REPRESENTATION_RELATIONSHIP()
);
#125=(
REPRESENTATION_RELATIONSHIP($,$,#6812,#6811)
REPRESENTATION_RELATIONSHIP_WITH_TRANSFORMATION(#66)
SHAPE_REPRESENTATION_RELATIONSHIP()
);
#126=(
REPRESENTATION_RELATIONSHIP($,$,#6816,#6811)
REPRESENTATION_RELATIONSHIP_WITH_TRANSFORMATION(#67)
SHAPE_REPRESENTATION_RELATIONSHIP()
);
#127=(
REPRESENTATION_RELATIONSHIP($,$,#6817,#6811)
REPRESENTATION_RELATIONSHIP_WITH_TRANSFORMATION(#68)
SHAPE_REPRESENTATION_RELATIONSHIP()
);
#128=(
REPRESENTATION_RELATIONSHIP($,$,#6827,#6811)
REPRESENTATION_RELATIONSHIP_WITH_TRANSFORMATION(#69)
SHAPE_REPRESENTATION_RELATIONSHIP()
);
#129=CONTEXT_DEPENDENT_SHAPE_REPRESENTATION(#70,#6745);
#130=CONTEXT_DEPENDENT_SHAPE_REPRESENTATION(#71,#6746);
#131=CONTEXT_DEPENDENT_SHAPE_REPRESENTATION(#72,#6747);
#132=CONTEXT_DEPENDENT_SHAPE_REPRESENTATION(#73,#6748);
#133=CONTEXT_DEPENDENT_SHAPE_REPRESENTATION(#74,#6749);
#134=CONTEXT_DEPENDENT_SHAPE_REPRESENTATION(#75,#6752);
#135=CONTEXT_DEPENDENT_SHAPE_REPRESENTATION(#76,#6753);
#136=CONTEXT_DEPENDENT_SHAPE_REPRESENTATION(#77,#6754);
#137=CONTEXT_DEPENDENT_SHAPE_REPRESENTATION(#78,#6755);
#138=CONTEXT_DEPENDENT_SHAPE_REPRESENTATION(#79,#6756);
#139=CONTEXT_DEPENDENT_SHAPE_REPRESENTATION(#80,#6757);
#140=CONTEXT_DEPENDENT_SHAPE_REPRESENTATION(#81,#6758);
#141=CONTEXT_DEPENDENT_SHAPE_REPRESENTATION(#82,#6759);
#142=CONTEXT_DEPENDENT_SHAPE_REPRESENTATION(#83,#6760);
#143=CONTEXT_DEPENDENT_SHAPE_REPRESENTATION(#84,#6761);
#144=CONTEXT_DEPENDENT_SHAPE_REPRESENTATION(#85,#6762);
#145=CONTEXT_DEPENDENT_SHAPE_REPRESENTATION(#86,#6763);
#146=CONTEXT_DEPENDENT_SHAPE_REPRESENTATION(#87,#6764);
#147=CONTEXT_DEPENDENT_SHAPE_REPRESENTATION(#88,#6765);
#148=CONTEXT_DEPENDENT_SHAPE_REPRESENTATION(#89,#6766);
#149=CONTEXT_DEPENDENT_SHAPE_REPRESENTATION(#90,#6767);
#150=CONTEXT_DEPENDENT_SHAPE_REPRESENTATION(#91,#6768);
#151=CONTEXT_DEPENDENT_SHAPE_REPRESENTATION(#92,#6769);
#152=CONTEXT_DEPENDENT_SHAPE_REPRESENTATION(#93,#6770);
#153=CONTEXT_DEPENDENT_SHAPE_REPRESENTATION(#94,#6771);
#154=CONTEXT_DEPENDENT_SHAPE_REPRESENTATION(#95,#6772);
#155=CONTEXT_DEPENDENT_SHAPE_REPRESENTATION(#96,#6773);
#156=CONTEXT_DEPENDENT_SHAPE_REPRESENTATION(#97,#6774);
#157=CONTEXT_DEPENDENT_SHAPE_REPRESENTATION(#98,#6780);
#158=CONTEXT_DEPENDENT_SHAPE_REPRESENTATION(#99,#6781);
#159=CONTEXT_DEPENDENT_SHAPE_REPRESENTATION(#100,#6782);
#160=CONTEXT_DEPENDENT_SHAPE_REPRESENTATION(#101,#6783);
#161=CONTEXT_DEPENDENT_SHAPE_REPRESENTATION(#102,#6784);
#162=CONTEXT_DEPENDENT_SHAPE_REPRESENTATION(#103,#6785);
#163=CONTEXT_DEPENDENT_SHAPE_REPRESENTATION(#104,#6786);
#164=CONTEXT_DEPENDENT_SHAPE_REPRESENTATION(#105,#6787);
#165=CONTEXT_DEPENDENT_SHAPE_REPRESENTATION(#106,#6788);
#166=CONTEXT_DEPENDENT_SHAPE_REPRESENTATION(#107,#6789);
#167=CONTEXT_DEPENDENT_SHAPE_REPRESENTATION(#108,#6790);
#168=CONTEXT_DEPENDENT_SHAPE_REPRESENTATION(#109,#6791);
#169=CONTEXT_DEPENDENT_SHAPE_REPRESENTATION(#110,#6792);
#170=CONTEXT_DEPENDENT_SHAPE_REPRESENTATION(#111,#6793);
#171=CONTEXT_DEPENDENT_SHAPE_REPRESENTATION(#112,#6794);
#172=CONTEXT_DEPENDENT_SHAPE_REPRESENTATION(#113,#6795);
#173=CONTEXT_DEPENDENT_SHAPE_REPRESENTATION(#114,#6796);
#174=CONTEXT_DEPENDENT_SHAPE_REPRESENTATION(#115,#6797);
#175=CONTEXT_DEPENDENT_SHAPE_REPRESENTATION(#116,#6798);
#176=CONTEXT_DEPENDENT_SHAPE_REPRESENTATION(#117,#6799);
#177=CONTEXT_DEPENDENT_SHAPE_REPRESENTATION(#118,#6800);
#178=CONTEXT_DEPENDENT_SHAPE_REPRESENTATION(#119,#6801);
#179=CONTEXT_DEPENDENT_SHAPE_REPRESENTATION(#120,#6802);
#180=CONTEXT_DEPENDENT_SHAPE_REPRESENTATION(#121,#6803);
#181=CONTEXT_DEPENDENT_SHAPE_REPRESENTATION(#122,#6804);
#182=CONTEXT_DEPENDENT_SHAPE_REPRESENTATION(#123,#6805);
#183=CONTEXT_DEPENDENT_SHAPE_REPRESENTATION(#124,#6806);
#184=CONTEXT_DEPENDENT_SHAPE_REPRESENTATION(#125,#6807);
#185=CONTEXT_DEPENDENT_SHAPE_REPRESENTATION(#126,#6808);
#186=CONTEXT_DEPENDENT_SHAPE_REPRESENTATION(#127,#6809);
#187=CONTEXT_DEPENDENT_SHAPE_REPRESENTATION(#128,#6810);
#188=NEXT_ASSEMBLY_USAGE_OCCURRENCE('Inner ring:1','Inner ring:1',
'Inner ring:1',#6841,#6842,'Inner ring:1');
#189=NEXT_ASSEMBLY_USAGE_OCCURRENCE('Outer ring:1','Outer ring:1',
'Outer ring:1',#6841,#6843,'Outer ring:1');
#190=NEXT_ASSEMBLY_USAGE_OCCURRENCE('Balls:1','Balls:1','Balls:1',#6841,
#6844,'Balls:1');
#191=NEXT_ASSEMBLY_USAGE_OCCURRENCE('Cage:1','Cage:1','Cage:1',#6841,#6845,
'Cage:1');
#192=NEXT_ASSEMBLY_USAGE_OCCURRENCE('Seals 2RS:1','Seals 2RS:1',
'Seals 2RS:1',#6841,#6846,'Seals 2RS:1');
#193=NEXT_ASSEMBLY_USAGE_OCCURRENCE('Tabletop base:1','Tabletop base:1',
'Tabletop base:1',#6834,#6835,'Tabletop base:1');
#194=NEXT_ASSEMBLY_USAGE_OCCURRENCE('Pivot pedestal:2',
'Pivot pedestal:2','Pivot pedestal:2',#6834,#6836,'Pivot pedestal:2');
#195=NEXT_ASSEMBLY_USAGE_OCCURRENCE('Pivot cap:2','Pivot cap:2',
'Pivot cap:2',#6834,#6847,'Pivot cap:2');
#196=NEXT_ASSEMBLY_USAGE_OCCURRENCE(
'Sealed Ball Bearing - 10 x 30 x 9 mm:2',
'Sealed Ball Bearing - 10 x 30 x 9 mm:2',
'Sealed Ball Bearing - 10 x 30 x 9 mm:2',#6834,#6841,
'Sealed Ball Bearing - 10 x 30 x 9 mm:2');
#197=NEXT_ASSEMBLY_USAGE_OCCURRENCE('M5x14 Cap Screw:2',
'M5x14 Cap Screw:2','M5x14 Cap Screw:2',#6834,#6837,'M5x14 Cap Screw:2');
#198=NEXT_ASSEMBLY_USAGE_OCCURRENCE('M5x14 Cap Screw:3',
'M5x14 Cap Screw:3','M5x14 Cap Screw:3',#6834,#6837,'M5x14 Cap Screw:3');
#199=NEXT_ASSEMBLY_USAGE_OCCURRENCE('M5x14 Cap Screw:4',
'M5x14 Cap Screw:4','M5x14 Cap Screw:4',#6834,#6837,'M5x14 Cap Screw:4');
#200=NEXT_ASSEMBLY_USAGE_OCCURRENCE('M5x14 Cap Screw:5',
'M5x14 Cap Screw:5','M5x14 Cap Screw:5',#6834,#6837,'M5x14 Cap Screw:5');
#201=NEXT_ASSEMBLY_USAGE_OCCURRENCE('M4x10 Cap Screw:2',
'M4x10 Cap Screw:2','M4x10 Cap Screw:2',#6834,#6848,'M4x10 Cap Screw:2');
#202=NEXT_ASSEMBLY_USAGE_OCCURRENCE('M4x10 Cap Screw:4',
'M4x10 Cap Screw:4','M4x10 Cap Screw:4',#6834,#6848,'M4x10 Cap Screw:4');
#203=NEXT_ASSEMBLY_USAGE_OCCURRENCE('M4x10 Cap Screw:6',
'M4x10 Cap Screw:6','M4x10 Cap Screw:6',#6834,#6848,'M4x10 Cap Screw:6');
#204=NEXT_ASSEMBLY_USAGE_OCCURRENCE('M4x10 Cap Screw:8',
'M4x10 Cap Screw:8','M4x10 Cap Screw:8',#6834,#6848,'M4x10 Cap Screw:8');
#205=NEXT_ASSEMBLY_USAGE_OCCURRENCE('Pivot pedestal:3',
'Pivot pedestal:3','Pivot pedestal:3',#6834,#6836,'Pivot pedestal:3');
#206=NEXT_ASSEMBLY_USAGE_OCCURRENCE('Pivot cap:4','Pivot cap:4',
'Pivot cap:4',#6834,#6847,'Pivot cap:4');
#207=NEXT_ASSEMBLY_USAGE_OCCURRENCE(
'Sealed Ball Bearing - 10 x 30 x 9 mm:4',
'Sealed Ball Bearing - 10 x 30 x 9 mm:4',
'Sealed Ball Bearing - 10 x 30 x 9 mm:4',#6834,#6841,
'Sealed Ball Bearing - 10 x 30 x 9 mm:4');
#208=NEXT_ASSEMBLY_USAGE_OCCURRENCE('M5x14 Cap Screw:6',
'M5x14 Cap Screw:6','M5x14 Cap Screw:6',#6834,#6837,'M5x14 Cap Screw:6');
#209=NEXT_ASSEMBLY_USAGE_OCCURRENCE('M5x14 Cap Screw:7',
'M5x14 Cap Screw:7','M5x14 Cap Screw:7',#6834,#6837,'M5x14 Cap Screw:7');
#210=NEXT_ASSEMBLY_USAGE_OCCURRENCE('M5x14 Cap Screw:8',
'M5x14 Cap Screw:8','M5x14 Cap Screw:8',#6834,#6837,'M5x14 Cap Screw:8');
#211=NEXT_ASSEMBLY_USAGE_OCCURRENCE('M5x14 Cap Screw:9',
'M5x14 Cap Screw:9','M5x14 Cap Screw:9',#6834,#6837,'M5x14 Cap Screw:9');
#212=NEXT_ASSEMBLY_USAGE_OCCURRENCE('M4x10 Cap Screw:10',
'M4x10 Cap Screw:10','M4x10 Cap Screw:10',#6834,#6848,
'M4x10 Cap Screw:10');
#213=NEXT_ASSEMBLY_USAGE_OCCURRENCE('M4x10 Cap Screw:12',
'M4x10 Cap Screw:12','M4x10 Cap Screw:12',#6834,#6848,
'M4x10 Cap Screw:12');
#214=NEXT_ASSEMBLY_USAGE_OCCURRENCE('M4x10 Cap Screw:14',
'M4x10 Cap Screw:14','M4x10 Cap Screw:14',#6834,#6848,
'M4x10 Cap Screw:14');
#215=NEXT_ASSEMBLY_USAGE_OCCURRENCE('M4x10 Cap Screw:16',
'M4x10 Cap Screw:16','M4x10 Cap Screw:16',#6834,#6848,
'M4x10 Cap Screw:16');
#216=NEXT_ASSEMBLY_USAGE_OCCURRENCE('Forty millimetre crank:1',
'Forty millimetre crank:1','Forty millimetre crank:1',#6838,#6840,
'Forty millimetre crank:1');
#217=NEXT_ASSEMBLY_USAGE_OCCURRENCE(
'Sealed Ball Bearing - 10 x 30 x 9 mm:3',
'Sealed Ball Bearing - 10 x 30 x 9 mm:3',
'Sealed Ball Bearing - 10 x 30 x 9 mm:3',#6838,#6841,
'Sealed Ball Bearing - 10 x 30 x 9 mm:3');
#218=NEXT_ASSEMBLY_USAGE_OCCURRENCE('Pivot cap:3','Pivot cap:3',
'Pivot cap:3',#6838,#6847,'Pivot cap:3');
#219=NEXT_ASSEMBLY_USAGE_OCCURRENCE('M4x10 Cap Screw:3',
'M4x10 Cap Screw:3','M4x10 Cap Screw:3',#6838,#6848,'M4x10 Cap Screw:3');
#220=NEXT_ASSEMBLY_USAGE_OCCURRENCE('M4x10 Cap Screw:5',
'M4x10 Cap Screw:5','M4x10 Cap Screw:5',#6838,#6848,'M4x10 Cap Screw:5');
#221=NEXT_ASSEMBLY_USAGE_OCCURRENCE('M4x10 Cap Screw:7',
'M4x10 Cap Screw:7','M4x10 Cap Screw:7',#6838,#6848,'M4x10 Cap Screw:7');
#222=NEXT_ASSEMBLY_USAGE_OCCURRENCE('M4x10 Cap Screw:9',
'M4x10 Cap Screw:9','M4x10 Cap Screw:9',#6838,#6848,'M4x10 Cap Screw:9');
#223=NEXT_ASSEMBLY_USAGE_OCCURRENCE('Lower race sleeve:2',
'Lower race sleeve:2','Lower race sleeve:2',#6838,#6851,
'Lower race sleeve:2');
#224=NEXT_ASSEMBLY_USAGE_OCCURRENCE('Spindle collar:2',
'Spindle collar:2','Spindle collar:2',#6838,#6852,'Spindle collar:2');
#225=NEXT_ASSEMBLY_USAGE_OCCURRENCE('M4x4 collar screw:2',
'M4x4 collar screw:2','M4x4 collar screw:2',#6838,#6853,
'M4x4 collar screw:2');
#226=NEXT_ASSEMBLY_USAGE_OCCURRENCE('Forty millimetre crank:2',
'Forty millimetre crank:2','Forty millimetre crank:2',#6839,#6840,
'Forty millimetre crank:2');
#227=NEXT_ASSEMBLY_USAGE_OCCURRENCE(
'Sealed Ball Bearing - 10 x 30 x 9 mm:5',
'Sealed Ball Bearing - 10 x 30 x 9 mm:5',
'Sealed Ball Bearing - 10 x 30 x 9 mm:5',#6839,#6841,
'Sealed Ball Bearing - 10 x 30 x 9 mm:5');
#228=NEXT_ASSEMBLY_USAGE_OCCURRENCE('Pivot cap:5','Pivot cap:5',
'Pivot cap:5',#6839,#6847,'Pivot cap:5');
#229=NEXT_ASSEMBLY_USAGE_OCCURRENCE('M4x10 Cap Screw:11',
'M4x10 Cap Screw:11','M4x10 Cap Screw:11',#6839,#6848,
'M4x10 Cap Screw:11');
#230=NEXT_ASSEMBLY_USAGE_OCCURRENCE('M4x10 Cap Screw:13',
'M4x10 Cap Screw:13','M4x10 Cap Screw:13',#6839,#6848,
'M4x10 Cap Screw:13');
#231=NEXT_ASSEMBLY_USAGE_OCCURRENCE('M4x10 Cap Screw:15',
'M4x10 Cap Screw:15','M4x10 Cap Screw:15',#6839,#6848,
'M4x10 Cap Screw:15');
#232=NEXT_ASSEMBLY_USAGE_OCCURRENCE('M4x10 Cap Screw:17',
'M4x10 Cap Screw:17','M4x10 Cap Screw:17',#6839,#6848,
'M4x10 Cap Screw:17');
#233=NEXT_ASSEMBLY_USAGE_OCCURRENCE('Lower race sleeve:4',
'Lower race sleeve:4','Lower race sleeve:4',#6839,#6851,
'Lower race sleeve:4');
#234=NEXT_ASSEMBLY_USAGE_OCCURRENCE('Spindle collar:4',
'Spindle collar:4','Spindle collar:4',#6839,#6852,'Spindle collar:4');
#235=NEXT_ASSEMBLY_USAGE_OCCURRENCE('M4x4 collar screw:4',
'M4x4 collar screw:4','M4x4 collar screw:4',#6839,#6853,
'M4x4 collar screw:4');
#236=NEXT_ASSEMBLY_USAGE_OCCURRENCE(
'Eighty millimetre coupler and pins:1',
'Eighty millimetre coupler and pins:1',
'Eighty millimetre coupler and pins:1',#6849,#6850,
'Eighty millimetre coupler and pins:1');
#237=NEXT_ASSEMBLY_USAGE_OCCURRENCE('Lower race sleeve:3',
'Lower race sleeve:3','Lower race sleeve:3',#6849,#6851,
'Lower race sleeve:3');
#238=NEXT_ASSEMBLY_USAGE_OCCURRENCE('Spindle collar:3',
'Spindle collar:3','Spindle collar:3',#6849,#6852,'Spindle collar:3');
#239=NEXT_ASSEMBLY_USAGE_OCCURRENCE('M4x4 collar screw:3',
'M4x4 collar screw:3','M4x4 collar screw:3',#6849,#6853,
'M4x4 collar screw:3');
#240=NEXT_ASSEMBLY_USAGE_OCCURRENCE('Lower race sleeve:5',
'Lower race sleeve:5','Lower race sleeve:5',#6849,#6851,
'Lower race sleeve:5');
#241=NEXT_ASSEMBLY_USAGE_OCCURRENCE('Spindle collar:5',
'Spindle collar:5','Spindle collar:5',#6849,#6852,'Spindle collar:5');
#242=NEXT_ASSEMBLY_USAGE_OCCURRENCE('M4x4 collar screw:5',
'M4x4 collar screw:5','M4x4 collar screw:5',#6849,#6853,
'M4x4 collar screw:5');
#243=NEXT_ASSEMBLY_USAGE_OCCURRENCE('Base and fixed pivots:1',
'Base and fixed pivots:1','Base and fixed pivots:1',#6833,#6834,
'Base and fixed pivots:1');
#244=NEXT_ASSEMBLY_USAGE_OCCURRENCE('First crank:1','First crank:1',
'First crank:1',#6833,#6838,'First crank:1');
#245=NEXT_ASSEMBLY_USAGE_OCCURRENCE('Second crank:1','Second crank:1',
'Second crank:1',#6833,#6839,'Second crank:1');
#246=NEXT_ASSEMBLY_USAGE_OCCURRENCE('Parallel coupler:1',
'Parallel coupler:1','Parallel coupler:1',#6833,#6849,
'Parallel coupler:1');
#247=SPHERICAL_SURFACE('',#3789,0.23815);
#248=SPHERICAL_SURFACE('',#3791,0.23815);
#249=SPHERICAL_SURFACE('',#3793,0.23815);
#250=SPHERICAL_SURFACE('',#3795,0.23815);
#251=SPHERICAL_SURFACE('',#3797,0.23815);
#252=SPHERICAL_SURFACE('',#3799,0.23815);
#253=SPHERICAL_SURFACE('',#3801,0.23815);
#254=SPHERICAL_SURFACE('',#3803,0.23815);
#255=SPHERICAL_SURFACE('',#3806,0.247676);
#256=SPHERICAL_SURFACE('',#3822,0.247676);
#257=SPHERICAL_SURFACE('',#3827,0.247676);
#258=SPHERICAL_SURFACE('',#3832,0.247676);
#259=SPHERICAL_SURFACE('',#3837,0.247676);
#260=SPHERICAL_SURFACE('',#3842,0.247676);
#261=SPHERICAL_SURFACE('',#3847,0.247676);
#262=SPHERICAL_SURFACE('',#3855,0.247676);
#263=TOROIDAL_SURFACE('',#3749,1.,0.247676);
#264=TOROIDAL_SURFACE('',#3769,1.,0.247676);
#265=CONICAL_SURFACE('',#3688,0.4,0.785398163397448);
#266=CONICAL_SURFACE('',#3692,0.41,0.785398163397448);
#267=CONICAL_SURFACE('',#3696,0.26,0.463647609000806);
#268=CONICAL_SURFACE('',#3760,0.53,0.785398163397448);
#269=CONICAL_SURFACE('',#3767,0.53,0.785398163397448);
#270=CONICAL_SURFACE('',#3780,1.47,0.785398163397449);
#271=CONICAL_SURFACE('',#3784,1.47,0.785398163397449);
#272=CONICAL_SURFACE('',#3935,0.325,0.785398163397448);
#273=CONICAL_SURFACE('',#3939,0.335,0.785398163397448);
#274=CONICAL_SURFACE('',#3943,0.21,0.463647609000806);
#275=CONICAL_SURFACE('',#4032,0.185,0.785398163397449);
#276=ORIENTED_CLOSED_SHELL('',*,#3383,.F.);
#277=ORIENTED_CLOSED_SHELL('',*,#3400,.F.);
#278=BREP_WITH_VOIDS('Body1',#3384,(#276));
#279=BREP_WITH_VOIDS('Body1',#3401,(#277));
#280=B_SPLINE_CURVE_WITH_KNOTS('',3,(#5305,#5306,#5307,#5308,#5309,#5310,
#5311,#5312,#5313,#5314),.UNSPECIFIED.,.F.,.F.,(4,2,2,2,4),(0.,0.0945941824764479,
0.189188364952896,0.283770357603024,0.378352350253152),.UNSPECIFIED.);
#281=B_SPLINE_CURVE_WITH_KNOTS('',3,(#5315,#5316,#5317,#5318,#5319,#5320,
#5321,#5322,#5323,#5324,#5325,#5326,#5327,#5328,#5329,#5330,#5331,#5332,
#5333,#5334,#5335,#5336,#5337,#5338,#5339,#5340),.UNSPECIFIED.,.F.,.F.,
(4,2,2,2,2,2,2,2,2,2,2,2,4),(0.378352350253152,0.47293434290328,0.567516335553408,
0.662110518029855,0.756704700506303,0.851298882982751,0.945893065459199,
1.04047505810933,1.13505705075946,1.22963904340958,1.32422103605971,1.41881521853616,
1.51340940101261),.UNSPECIFIED.);
#282=B_SPLINE_CURVE_WITH_KNOTS('',3,(#5344,#5345,#5346,#5347,#5348,#5349,
#5350,#5351,#5352,#5353,#5354,#5355,#5356,#5357,#5358,#5359,#5360,#5361,
#5362,#5363,#5364,#5365,#5366,#5367,#5368,#5369),.UNSPECIFIED.,.F.,.F.,
(4,2,2,2,2,2,2,2,2,2,2,2,4),(0.,0.0942186410044058,0.188437282008812,0.282655768798837,
0.376874255588861,0.471092742378886,0.565311229168911,0.659529870173317,
0.753748511177723,0.847967152182129,0.942185793186535,1.03640427997656,
1.13062276676658),.UNSPECIFIED.);
#283=B_SPLINE_CURVE_WITH_KNOTS('',3,(#5370,#5371,#5372,#5373,#5374,#5375,
#5376,#5377,#5378,#5379),.UNSPECIFIED.,.F.,.F.,(4,2,2,2,4),(1.13062276676658,
1.22484125355661,1.31905974034663,1.41327838135104,1.50749702235545),
 .UNSPECIFIED.);
#284=B_SPLINE_CURVE_WITH_KNOTS('',3,(#5773,#5774,#5775,#5776,#5777,#5778,
#5779,#5780,#5781,#5782,#5783,#5784,#5785,#5786,#5787,#5788,#5789,#5790,
#5791,#5792,#5793,#5794),.UNSPECIFIED.,.F.,.F.,(4,2,2,2,2,2,2,2,2,2,4),
(0.0473477652366656,0.126350602536658,0.189525903804987,0.252701205073317,
0.313298422430275,0.373895639787233,0.434492857144191,0.495090074501149,
0.558265375769478,0.621440677037807,0.7004435143378),.UNSPECIFIED.);
#285=B_SPLINE_CURVE_WITH_KNOTS('',3,(#5798,#5799,#5800,#5801,#5802,#5803,
#5804,#5805,#5806,#5807,#5808,#5809,#5810,#5811,#5812,#5813,#5814,#5815,
#5816,#5817,#5818,#5819),.UNSPECIFIED.,.F.,.F.,(4,2,2,2,2,2,2,2,2,2,4),
(0.0464897534940957,0.0852567806515119,0.170513561303024,0.246687263103517,
0.308657850341199,0.370628437578881,0.432599024816563,0.494569612054245,
0.570743313854739,0.656000094506251,0.694767121663666),.UNSPECIFIED.);
#286=B_SPLINE_CURVE_WITH_KNOTS('',3,(#5825,#5826,#5827,#5828,#5829,#5830,
#5831,#5832,#5833,#5834,#5835,#5836,#5837,#5838,#5839,#5840,#5841,#5842,
#5843,#5844,#5845,#5846),.UNSPECIFIED.,.F.,.F.,(4,2,2,2,2,2,2,2,2,2,4),
(0.0464897534940957,0.0852567806515118,0.170513561303024,0.246687263103517,
0.308657850341199,0.370628437578881,0.432599024816563,0.494569612054245,
0.570743313854738,0.65600009450625,0.694767121663666),.UNSPECIFIED.);
#287=B_SPLINE_CURVE_WITH_KNOTS('',3,(#5850,#5851,#5852,#5853,#5854,#5855,
#5856,#5857,#5858,#5859,#5860,#5861,#5862,#5863,#5864,#5865,#5866,#5867,
#5868,#5869,#5870,#5871),.UNSPECIFIED.,.F.,.F.,(4,2,2,2,2,2,2,2,2,2,4),
(0.0464897534940957,0.0852567806515119,0.170513561303024,0.246687263103517,
0.308657850341199,0.370628437578881,0.432599024816563,0.494569612054245,
0.570743313854739,0.656000094506251,0.694767121663666),.UNSPECIFIED.);
#288=B_SPLINE_CURVE_WITH_KNOTS('',3,(#5875,#5876,#5877,#5878,#5879,#5880,
#5881,#5882,#5883,#5884,#5885,#5886),.UNSPECIFIED.,.F.,.F.,(4,2,2,2,2,4),
(0.0464897534940957,0.0852567806515119,0.170513561303024,0.246687263103517,
0.308657850341199,0.370628437578881),.UNSPECIFIED.);
#289=B_SPLINE_CURVE_WITH_KNOTS('',3,(#5891,#5892,#5893,#5894,#5895,#5896,
#5897,#5898,#5899,#5900,#5901,#5902),.UNSPECIFIED.,.F.,.F.,(4,2,2,2,2,4),
(0.370628437578881,0.432599024816563,0.494569612054245,0.570743313854738,
0.65600009450625,0.694767121663666),.UNSPECIFIED.);
#290=B_SPLINE_CURVE_WITH_KNOTS('',3,(#5906,#5907,#5908,#5909,#5910,#5911,
#5912,#5913,#5914,#5915,#5916,#5917,#5918,#5919,#5920,#5921,#5922,#5923,
#5924,#5925,#5926,#5927),.UNSPECIFIED.,.F.,.F.,(4,2,2,2,2,2,2,2,2,2,4),
(0.0464897534940957,0.0852567806515121,0.170513561303024,0.246687263103518,
0.308657850341199,0.370628437578881,0.432599024816563,0.494569612054245,
0.570743313854738,0.65600009450625,0.694767121663666),.UNSPECIFIED.);
#291=B_SPLINE_CURVE_WITH_KNOTS('',3,(#5931,#5932,#5933,#5934,#5935,#5936,
#5937,#5938,#5939,#5940,#5941,#5942,#5943,#5944,#5945,#5946,#5947,#5948,
#5949,#5950,#5951,#5952),.UNSPECIFIED.,.F.,.F.,(4,2,2,2,2,2,2,2,2,2,4),
(0.0464897534940957,0.0852567806515119,0.170513561303024,0.246687263103517,
0.308657850341199,0.370628437578881,0.432599024816563,0.494569612054245,
0.570743313854738,0.65600009450625,0.694767121663667),.UNSPECIFIED.);
#292=B_SPLINE_CURVE_WITH_KNOTS('',3,(#5956,#5957,#5958,#5959,#5960,#5961,
#5962,#5963,#5964,#5965,#5966,#5967,#5968,#5969,#5970,#5971,#5972,#5973,
#5974,#5975,#5976,#5977),.UNSPECIFIED.,.F.,.F.,(4,2,2,2,2,2,2,2,2,2,4),
(0.0464897534940957,0.0852567806515119,0.170513561303024,0.246687263103517,
0.308657850341199,0.370628437578881,0.432599024816563,0.494569612054245,
0.570743313854738,0.65600009450625,0.694767121663666),.UNSPECIFIED.);
#293=B_SPLINE_CURVE_WITH_KNOTS('',3,(#5981,#5982,#5983,#5984,#5985,#5986,
#5987,#5988,#5989,#5990,#5991,#5992,#5993,#5994,#5995,#5996,#5997,#5998,
#5999,#6000,#6001,#6002),.UNSPECIFIED.,.F.,.F.,(4,2,2,2,2,2,2,2,2,2,4),
(0.0464897534940957,0.0852567806515119,0.170513561303024,0.246687263103517,
0.308657850341199,0.370628437578881,0.432599024816563,0.494569612054245,
0.570743313854739,0.656000094506251,0.694767121663667),.UNSPECIFIED.);
#294=B_SPLINE_CURVE_WITH_KNOTS('',3,(#6010,#6011,#6012,#6013,#6014,#6015,
#6016,#6017,#6018,#6019,#6020,#6021,#6022,#6023,#6024,#6025,#6026,#6027,
#6028,#6029,#6030,#6031),.UNSPECIFIED.,.F.,.F.,(4,2,2,2,2,2,2,2,2,2,4),
(0.0473477652366656,0.126350602536658,0.189525903804987,0.252701205073316,
0.313298422430274,0.373895639787232,0.434492857144191,0.495090074501149,
0.558265375769478,0.621440677037807,0.7004435143378),.UNSPECIFIED.);
#295=B_SPLINE_CURVE_WITH_KNOTS('',3,(#6039,#6040,#6041,#6042,#6043,#6044,
#6045,#6046,#6047,#6048,#6049,#6050,#6051,#6052,#6053,#6054,#6055,#6056,
#6057,#6058,#6059,#6060),.UNSPECIFIED.,.F.,.F.,(4,2,2,2,2,2,2,2,2,2,4),
(0.0473477652366656,0.126350602536658,0.189525903804987,0.252701205073317,
0.313298422430275,0.373895639787233,0.434492857144191,0.495090074501149,
0.558265375769478,0.621440677037807,0.7004435143378),.UNSPECIFIED.);
#296=B_SPLINE_CURVE_WITH_KNOTS('',3,(#6069,#6070,#6071,#6072,#6073,#6074,
#6075,#6076,#6077,#6078,#6079,#6080),.UNSPECIFIED.,.F.,.F.,(4,2,2,2,2,4),
(0.0473477652366656,0.126350602536658,0.189525903804987,0.252701205073316,
0.313298422430275,0.373895639787233),.UNSPECIFIED.);
#297=B_SPLINE_CURVE_WITH_KNOTS('',3,(#6082,#6083,#6084,#6085,#6086,#6087,
#6088,#6089,#6090,#6091,#6092,#6093),.UNSPECIFIED.,.F.,.F.,(4,2,2,2,2,4),
(0.373895639787233,0.434492857144191,0.495090074501149,0.558265375769478,
0.621440677037807,0.7004435143378),.UNSPECIFIED.);
#298=B_SPLINE_CURVE_WITH_KNOTS('',3,(#6100,#6101,#6102,#6103,#6104,#6105,
#6106,#6107,#6108,#6109,#6110,#6111,#6112,#6113,#6114,#6115,#6116,#6117,
#6118,#6119,#6120,#6121),.UNSPECIFIED.,.F.,.F.,(4,2,2,2,2,2,2,2,2,2,4),
(0.0473477652366656,0.126350602536658,0.189525903804987,0.252701205073316,
0.313298422430275,0.373895639787233,0.434492857144191,0.495090074501149,
0.558265375769478,0.621440677037807,0.7004435143378),.UNSPECIFIED.);
#299=B_SPLINE_CURVE_WITH_KNOTS('',3,(#6129,#6130,#6131,#6132,#6133,#6134,
#6135,#6136,#6137,#6138,#6139,#6140,#6141,#6142,#6143,#6144,#6145,#6146,
#6147,#6148,#6149,#6150),.UNSPECIFIED.,.F.,.F.,(4,2,2,2,2,2,2,2,2,2,4),
(0.0473477652366656,0.126350602536658,0.189525903804987,0.252701205073317,
0.313298422430275,0.373895639787233,0.434492857144191,0.495090074501149,
0.558265375769478,0.621440677037807,0.7004435143378),.UNSPECIFIED.);
#300=B_SPLINE_CURVE_WITH_KNOTS('',3,(#6158,#6159,#6160,#6161,#6162,#6163,
#6164,#6165,#6166,#6167,#6168,#6169,#6170,#6171,#6172,#6173,#6174,#6175,
#6176,#6177,#6178,#6179),.UNSPECIFIED.,.F.,.F.,(4,2,2,2,2,2,2,2,2,2,4),
(0.0473477652366656,0.126350602536658,0.189525903804987,0.252701205073316,
0.313298422430275,0.373895639787233,0.434492857144191,0.495090074501149,
0.558265375769478,0.621440677037807,0.7004435143378),.UNSPECIFIED.);
#301=B_SPLINE_CURVE_WITH_KNOTS('',3,(#6188,#6189,#6190,#6191,#6192,#6193,
#6194,#6195,#6196,#6197,#6198,#6199,#6200,#6201,#6202,#6203,#6204,#6205,
#6206,#6207,#6208,#6209),.UNSPECIFIED.,.F.,.F.,(4,2,2,2,2,2,2,2,2,2,4),
(0.0473477652366656,0.126350602536658,0.189525903804987,0.252701205073317,
0.313298422430275,0.373895639787233,0.434492857144191,0.495090074501149,
0.558265375769478,0.621440677037807,0.7004435143378),.UNSPECIFIED.);
#302=B_SPLINE_CURVE_WITH_KNOTS('',3,(#6493,#6494,#6495,#6496,#6497,#6498,
#6499,#6500,#6501,#6502,#6503,#6504,#6505,#6506),.UNSPECIFIED.,.F.,.F.,
(4,2,2,2,2,2,4),(0.618551524396293,0.626563103102765,0.689203386094988,
0.751843669087211,0.814483952079434,0.877124235071657,0.88513581377813),
 .UNSPECIFIED.);
#303=B_SPLINE_CURVE_WITH_KNOTS('',3,(#6510,#6511,#6512,#6513,#6514,#6515,
#6516,#6517),.UNSPECIFIED.,.F.,.F.,(4,2,2,4),(0.250614556362404,0.313254839354627,
0.37589512234685,0.383906701053323),.UNSPECIFIED.);
#304=B_SPLINE_CURVE_WITH_KNOTS('',3,(#6521,#6522,#6523,#6524,#6525,#6526,
#6527,#6528,#6529,#6530,#6531,#6532,#6533,#6534,#6535,#6536,#6537,#6538,
#6539,#6540,#6541,#6542,#6543,#6544,#6545,#6546),.UNSPECIFIED.,.F.,.F.,
(4,2,2,2,2,2,2,2,2,2,2,2,4),(0.,0.0623062782223143,0.124612556444629,0.186916384615149,
0.249220212785669,0.31152404095619,0.37382786912671,0.436134147349024,0.498440425571339,
0.560746703793653,0.623052982015967,0.685356810186488,0.747660638357008),
 .UNSPECIFIED.);
#305=B_SPLINE_CURVE_WITH_KNOTS('',3,(#6547,#6548,#6549,#6550,#6551,#6552,
#6553,#6554,#6555,#6556),.UNSPECIFIED.,.F.,.F.,(4,2,2,2,4),(0.747660638357008,
0.809964466527528,0.872268294698049,0.934574572920363,0.996880851142677),
 .UNSPECIFIED.);
#306=B_SPLINE_CURVE_WITH_KNOTS('',3,(#6557,#6558,#6559,#6560,#6561,#6562,
#6563,#6564),.UNSPECIFIED.,.F.,.F.,(4,2,2,4),(0.117322411671485,0.125333990377958,
0.187974273370181,0.250614556362404),.UNSPECIFIED.);
#307=SHAPE_REPRESENTATION_RELATIONSHIP('SRR','None',#6813,#322);
#308=SHAPE_REPRESENTATION_RELATIONSHIP('SRR','None',#6814,#323);
#309=SHAPE_REPRESENTATION_RELATIONSHIP('SRR','None',#6815,#324);
#310=SHAPE_REPRESENTATION_RELATIONSHIP('SRR','None',#6818,#325);
#311=SHAPE_REPRESENTATION_RELATIONSHIP('SRR','None',#6820,#326);
#312=SHAPE_REPRESENTATION_RELATIONSHIP('SRR','None',#6821,#327);
#313=SHAPE_REPRESENTATION_RELATIONSHIP('SRR','None',#6822,#328);
#314=SHAPE_REPRESENTATION_RELATIONSHIP('SRR','None',#6823,#329);
#315=SHAPE_REPRESENTATION_RELATIONSHIP('SRR','None',#6824,#330);
#316=SHAPE_REPRESENTATION_RELATIONSHIP('SRR','None',#6825,#331);
#317=SHAPE_REPRESENTATION_RELATIONSHIP('SRR','None',#6826,#332);
#318=SHAPE_REPRESENTATION_RELATIONSHIP('SRR','None',#6828,#333);
#319=SHAPE_REPRESENTATION_RELATIONSHIP('SRR','None',#6829,#334);
#320=SHAPE_REPRESENTATION_RELATIONSHIP('SRR','None',#6830,#335);
#321=SHAPE_REPRESENTATION_RELATIONSHIP('SRR','None',#6831,#336);
#322=ADVANCED_BREP_SHAPE_REPRESENTATION('',(#360),#6686);
#323=ADVANCED_BREP_SHAPE_REPRESENTATION('',(#361),#6687);
#324=ADVANCED_BREP_SHAPE_REPRESENTATION('',(#278),#6688);
#325=ADVANCED_BREP_SHAPE_REPRESENTATION('',(#362),#6691);
#326=ADVANCED_BREP_SHAPE_REPRESENTATION('',(#363),#6693);
#327=ADVANCED_BREP_SHAPE_REPRESENTATION('',(#364),#6694);
#328=ADVANCED_BREP_SHAPE_REPRESENTATION('',(#365,#366,#367,#368,#369,#370,
#371,#372),#6695);
#329=ADVANCED_BREP_SHAPE_REPRESENTATION('',(#373),#6696);
#330=ADVANCED_BREP_SHAPE_REPRESENTATION('',(#374,#375),#6697);
#331=ADVANCED_BREP_SHAPE_REPRESENTATION('',(#376),#6698);
#332=ADVANCED_BREP_SHAPE_REPRESENTATION('',(#279),#6699);
#333=ADVANCED_BREP_SHAPE_REPRESENTATION('',(#377),#6701);
#334=ADVANCED_BREP_SHAPE_REPRESENTATION('',(#378),#6702);
#335=ADVANCED_BREP_SHAPE_REPRESENTATION('',(#379),#6703);
#336=ADVANCED_BREP_SHAPE_REPRESENTATION('',(#380),#6704);
#337=STYLED_ITEM('',(#6968),#360);
#338=STYLED_ITEM('',(#7003),#361);
#339=STYLED_ITEM('',(#6996),#278);
#340=STYLED_ITEM('',(#7003),#362);
#341=STYLED_ITEM('',(#6989),#363);
#342=STYLED_ITEM('',(#6989),#364);
#343=STYLED_ITEM('',(#6989),#365);
#344=STYLED_ITEM('',(#6989),#366);
#345=STYLED_ITEM('',(#6989),#367);
#346=STYLED_ITEM('',(#6989),#368);
#347=STYLED_ITEM('',(#6989),#369);
#348=STYLED_ITEM('',(#6989),#370);
#349=STYLED_ITEM('',(#6989),#371);
#350=STYLED_ITEM('',(#6989),#372);
#351=STYLED_ITEM('',(#6989),#373);
#352=STYLED_ITEM('',(#6989),#374);
#353=STYLED_ITEM('',(#6989),#375);
#354=STYLED_ITEM('',(#6975),#376);
#355=STYLED_ITEM('',(#6996),#279);
#356=STYLED_ITEM('',(#6982),#377);
#357=STYLED_ITEM('',(#6975),#378);
#358=STYLED_ITEM('',(#6982),#379);
#359=STYLED_ITEM('',(#6996),#380);
#360=MANIFOLD_SOLID_BREP('Body1',#3381);
#361=MANIFOLD_SOLID_BREP('Body1',#3382);
#362=MANIFOLD_SOLID_BREP('Body1',#3385);
#363=MANIFOLD_SOLID_BREP('Body1',#3386);
#364=MANIFOLD_SOLID_BREP('Body1',#3387);
#365=MANIFOLD_SOLID_BREP('Body1',#3388);
#366=MANIFOLD_SOLID_BREP('Body2',#3389);
#367=MANIFOLD_SOLID_BREP('Body3',#3390);
#368=MANIFOLD_SOLID_BREP('Body4',#3391);
#369=MANIFOLD_SOLID_BREP('Body5',#3392);
#370=MANIFOLD_SOLID_BREP('Body6',#3393);
#371=MANIFOLD_SOLID_BREP('Body7',#3394);
#372=MANIFOLD_SOLID_BREP('Body8',#3395);
#373=MANIFOLD_SOLID_BREP('Continuous crown cage',#3396);
#374=MANIFOLD_SOLID_BREP('Body1',#3397);
#375=MANIFOLD_SOLID_BREP('Body2',#3398);
#376=MANIFOLD_SOLID_BREP('Body1',#3399);
#377=MANIFOLD_SOLID_BREP('Body1',#3402);
#378=MANIFOLD_SOLID_BREP('Body1',#3403);
#379=MANIFOLD_SOLID_BREP('Body1',#3404);
#380=MANIFOLD_SOLID_BREP('Body1',#3405);
#381=FACE_BOUND('',#778,.T.);
#382=FACE_BOUND('',#779,.T.);
#383=FACE_BOUND('',#780,.T.);
#384=FACE_BOUND('',#781,.T.);
#385=FACE_BOUND('',#782,.T.);
#386=FACE_BOUND('',#783,.T.);
#387=FACE_BOUND('',#784,.T.);
#388=FACE_BOUND('',#785,.T.);
#389=FACE_BOUND('',#787,.T.);
#390=FACE_BOUND('',#788,.T.);
#391=FACE_BOUND('',#789,.T.);
#392=FACE_BOUND('',#790,.T.);
#393=FACE_BOUND('',#791,.T.);
#394=FACE_BOUND('',#792,.T.);
#395=FACE_BOUND('',#793,.T.);
#396=FACE_BOUND('',#794,.T.);
#397=FACE_BOUND('',#814,.T.);
#398=FACE_BOUND('',#815,.T.);
#399=FACE_BOUND('',#816,.T.);
#400=FACE_BOUND('',#817,.T.);
#401=FACE_BOUND('',#818,.T.);
#402=FACE_BOUND('',#825,.T.);
#403=FACE_BOUND('',#827,.T.);
#404=FACE_BOUND('',#829,.T.);
#405=FACE_BOUND('',#831,.T.);
#406=FACE_BOUND('',#832,.T.);
#407=FACE_BOUND('',#833,.T.);
#408=FACE_BOUND('',#834,.T.);
#409=FACE_BOUND('',#835,.T.);
#410=FACE_BOUND('',#837,.T.);
#411=FACE_BOUND('',#838,.T.);
#412=FACE_BOUND('',#839,.T.);
#413=FACE_BOUND('',#840,.T.);
#414=FACE_BOUND('',#841,.T.);
#415=FACE_BOUND('',#856,.T.);
#416=FACE_BOUND('',#869,.T.);
#417=FACE_BOUND('',#872,.T.);
#418=FACE_BOUND('',#874,.T.);
#419=FACE_BOUND('',#875,.T.);
#420=FACE_BOUND('',#876,.T.);
#421=FACE_BOUND('',#877,.T.);
#422=FACE_BOUND('',#878,.T.);
#423=FACE_BOUND('',#880,.T.);
#424=FACE_BOUND('',#886,.T.);
#425=FACE_BOUND('',#888,.T.);
#426=FACE_BOUND('',#897,.T.);
#427=FACE_BOUND('',#900,.T.);
#428=FACE_BOUND('',#905,.T.);
#429=FACE_BOUND('',#910,.T.);
#430=FACE_BOUND('',#938,.T.);
#431=FACE_BOUND('',#941,.T.);
#432=FACE_BOUND('',#944,.T.);
#433=FACE_BOUND('',#947,.T.);
#434=FACE_BOUND('',#950,.T.);
#435=FACE_BOUND('',#954,.T.);
#436=FACE_BOUND('',#957,.T.);
#437=FACE_BOUND('',#960,.T.);
#438=FACE_BOUND('',#963,.T.);
#439=FACE_BOUND('',#970,.T.);
#440=FACE_BOUND('',#974,.T.);
#441=FACE_BOUND('',#975,.T.);
#442=FACE_BOUND('',#976,.T.);
#443=FACE_BOUND('',#977,.T.);
#444=FACE_BOUND('',#978,.T.);
#445=FACE_BOUND('',#980,.T.);
#446=FACE_BOUND('',#981,.T.);
#447=FACE_BOUND('',#982,.T.);
#448=FACE_BOUND('',#983,.T.);
#449=FACE_BOUND('',#984,.T.);
#450=FACE_BOUND('',#999,.T.);
#451=FACE_BOUND('',#1005,.T.);
#452=FACE_BOUND('',#1006,.T.);
#453=FACE_BOUND('',#1008,.T.);
#454=FACE_BOUND('',#1015,.T.);
#455=FACE_BOUND('',#1023,.T.);
#456=FACE_BOUND('',#1025,.T.);
#457=FACE_BOUND('',#1030,.T.);
#458=FACE_BOUND('',#1032,.T.);
#459=FACE_BOUND('',#1034,.T.);
#460=FACE_BOUND('',#1036,.T.);
#461=FACE_BOUND('',#1046,.T.);
#462=PLANE('',#3599);
#463=PLANE('',#3600);
#464=PLANE('',#3601);
#465=PLANE('',#3602);
#466=PLANE('',#3603);
#467=PLANE('',#3604);
#468=PLANE('',#3610);
#469=PLANE('',#3614);
#470=PLANE('',#3618);
#471=PLANE('',#3622);
#472=PLANE('',#3623);
#473=PLANE('',#3631);
#474=PLANE('',#3636);
#475=PLANE('',#3641);
#476=PLANE('',#3650);
#477=PLANE('',#3667);
#478=PLANE('',#3673);
#479=PLANE('',#3674);
#480=PLANE('',#3676);
#481=PLANE('',#3677);
#482=PLANE('',#3678);
#483=PLANE('',#3679);
#484=PLANE('',#3680);
#485=PLANE('',#3681);
#486=PLANE('',#3682);
#487=PLANE('',#3683);
#488=PLANE('',#3684);
#489=PLANE('',#3686);
#490=PLANE('',#3694);
#491=PLANE('',#3705);
#492=PLANE('',#3709);
#493=PLANE('',#3713);
#494=PLANE('',#3717);
#495=PLANE('',#3721);
#496=PLANE('',#3730);
#497=PLANE('',#3731);
#498=PLANE('',#3732);
#499=PLANE('',#3733);
#500=PLANE('',#3735);
#501=PLANE('',#3738);
#502=PLANE('',#3740);
#503=PLANE('',#3746);
#504=PLANE('',#3762);
#505=PLANE('',#3765);
#506=PLANE('',#3777);
#507=PLANE('',#3786);
#508=PLANE('',#3819);
#509=PLANE('',#3824);
#510=PLANE('',#3829);
#511=PLANE('',#3834);
#512=PLANE('',#3839);
#513=PLANE('',#3844);
#514=PLANE('',#3853);
#515=PLANE('',#3857);
#516=PLANE('',#3858);
#517=PLANE('',#3860);
#518=PLANE('',#3865);
#519=PLANE('',#3868);
#520=PLANE('',#3873);
#521=PLANE('',#3885);
#522=PLANE('',#3890);
#523=PLANE('',#3895);
#524=PLANE('',#3900);
#525=PLANE('',#3913);
#526=PLANE('',#3920);
#527=PLANE('',#3921);
#528=PLANE('',#3923);
#529=PLANE('',#3924);
#530=PLANE('',#3925);
#531=PLANE('',#3926);
#532=PLANE('',#3927);
#533=PLANE('',#3928);
#534=PLANE('',#3929);
#535=PLANE('',#3930);
#536=PLANE('',#3931);
#537=PLANE('',#3933);
#538=PLANE('',#3941);
#539=PLANE('',#3974);
#540=PLANE('',#3975);
#541=PLANE('',#3979);
#542=PLANE('',#3985);
#543=PLANE('',#3986);
#544=PLANE('',#3989);
#545=PLANE('',#3995);
#546=PLANE('',#3996);
#547=PLANE('',#4004);
#548=PLANE('',#4005);
#549=PLANE('',#4007);
#550=PLANE('',#4011);
#551=PLANE('',#4018);
#552=PLANE('',#4019);
#553=PLANE('',#4021);
#554=PLANE('',#4023);
#555=PLANE('',#4024);
#556=PLANE('',#4025);
#557=PLANE('',#4026);
#558=PLANE('',#4027);
#559=PLANE('',#4028);
#560=PLANE('',#4029);
#561=PLANE('',#4030);
#562=FACE_OUTER_BOUND('',#765,.T.);
#563=FACE_OUTER_BOUND('',#766,.T.);
#564=FACE_OUTER_BOUND('',#767,.T.);
#565=FACE_OUTER_BOUND('',#768,.T.);
#566=FACE_OUTER_BOUND('',#769,.T.);
#567=FACE_OUTER_BOUND('',#770,.T.);
#568=FACE_OUTER_BOUND('',#771,.T.);
#569=FACE_OUTER_BOUND('',#772,.T.);
#570=FACE_OUTER_BOUND('',#773,.T.);
#571=FACE_OUTER_BOUND('',#774,.T.);
#572=FACE_OUTER_BOUND('',#775,.T.);
#573=FACE_OUTER_BOUND('',#776,.T.);
#574=FACE_OUTER_BOUND('',#777,.T.);
#575=FACE_OUTER_BOUND('',#786,.T.);
#576=FACE_OUTER_BOUND('',#795,.T.);
#577=FACE_OUTER_BOUND('',#796,.T.);
#578=FACE_OUTER_BOUND('',#797,.T.);
#579=FACE_OUTER_BOUND('',#798,.T.);
#580=FACE_OUTER_BOUND('',#799,.T.);
#581=FACE_OUTER_BOUND('',#800,.T.);
#582=FACE_OUTER_BOUND('',#801,.T.);
#583=FACE_OUTER_BOUND('',#802,.T.);
#584=FACE_OUTER_BOUND('',#803,.T.);
#585=FACE_OUTER_BOUND('',#804,.T.);
#586=FACE_OUTER_BOUND('',#805,.T.);
#587=FACE_OUTER_BOUND('',#806,.T.);
#588=FACE_OUTER_BOUND('',#807,.T.);
#589=FACE_OUTER_BOUND('',#808,.T.);
#590=FACE_OUTER_BOUND('',#809,.T.);
#591=FACE_OUTER_BOUND('',#810,.T.);
#592=FACE_OUTER_BOUND('',#811,.T.);
#593=FACE_OUTER_BOUND('',#812,.T.);
#594=FACE_OUTER_BOUND('',#813,.T.);
#595=FACE_OUTER_BOUND('',#819,.T.);
#596=FACE_OUTER_BOUND('',#820,.T.);
#597=FACE_OUTER_BOUND('',#821,.T.);
#598=FACE_OUTER_BOUND('',#822,.T.);
#599=FACE_OUTER_BOUND('',#823,.T.);
#600=FACE_OUTER_BOUND('',#824,.T.);
#601=FACE_OUTER_BOUND('',#826,.T.);
#602=FACE_OUTER_BOUND('',#828,.T.);
#603=FACE_OUTER_BOUND('',#830,.T.);
#604=FACE_OUTER_BOUND('',#836,.T.);
#605=FACE_OUTER_BOUND('',#842,.T.);
#606=FACE_OUTER_BOUND('',#843,.T.);
#607=FACE_OUTER_BOUND('',#844,.T.);
#608=FACE_OUTER_BOUND('',#845,.T.);
#609=FACE_OUTER_BOUND('',#846,.T.);
#610=FACE_OUTER_BOUND('',#847,.T.);
#611=FACE_OUTER_BOUND('',#848,.T.);
#612=FACE_OUTER_BOUND('',#849,.T.);
#613=FACE_OUTER_BOUND('',#850,.T.);
#614=FACE_OUTER_BOUND('',#851,.T.);
#615=FACE_OUTER_BOUND('',#852,.T.);
#616=FACE_OUTER_BOUND('',#853,.T.);
#617=FACE_OUTER_BOUND('',#854,.T.);
#618=FACE_OUTER_BOUND('',#855,.T.);
#619=FACE_OUTER_BOUND('',#857,.T.);
#620=FACE_OUTER_BOUND('',#858,.T.);
#621=FACE_OUTER_BOUND('',#859,.T.);
#622=FACE_OUTER_BOUND('',#860,.T.);
#623=FACE_OUTER_BOUND('',#861,.T.);
#624=FACE_OUTER_BOUND('',#862,.T.);
#625=FACE_OUTER_BOUND('',#863,.T.);
#626=FACE_OUTER_BOUND('',#864,.T.);
#627=FACE_OUTER_BOUND('',#865,.T.);
#628=FACE_OUTER_BOUND('',#866,.T.);
#629=FACE_OUTER_BOUND('',#867,.T.);
#630=FACE_OUTER_BOUND('',#868,.T.);
#631=FACE_OUTER_BOUND('',#870,.T.);
#632=FACE_OUTER_BOUND('',#871,.T.);
#633=FACE_OUTER_BOUND('',#873,.T.);
#634=FACE_OUTER_BOUND('',#879,.T.);
#635=FACE_OUTER_BOUND('',#881,.T.);
#636=FACE_OUTER_BOUND('',#882,.T.);
#637=FACE_OUTER_BOUND('',#883,.T.);
#638=FACE_OUTER_BOUND('',#884,.T.);
#639=FACE_OUTER_BOUND('',#885,.T.);
#640=FACE_OUTER_BOUND('',#887,.T.);
#641=FACE_OUTER_BOUND('',#889,.T.);
#642=FACE_OUTER_BOUND('',#890,.T.);
#643=FACE_OUTER_BOUND('',#891,.T.);
#644=FACE_OUTER_BOUND('',#892,.T.);
#645=FACE_OUTER_BOUND('',#893,.T.);
#646=FACE_OUTER_BOUND('',#894,.T.);
#647=FACE_OUTER_BOUND('',#895,.T.);
#648=FACE_OUTER_BOUND('',#896,.T.);
#649=FACE_OUTER_BOUND('',#898,.T.);
#650=FACE_OUTER_BOUND('',#899,.T.);
#651=FACE_OUTER_BOUND('',#901,.T.);
#652=FACE_OUTER_BOUND('',#902,.T.);
#653=FACE_OUTER_BOUND('',#903,.T.);
#654=FACE_OUTER_BOUND('',#904,.T.);
#655=FACE_OUTER_BOUND('',#906,.T.);
#656=FACE_OUTER_BOUND('',#907,.T.);
#657=FACE_OUTER_BOUND('',#908,.T.);
#658=FACE_OUTER_BOUND('',#909,.T.);
#659=FACE_OUTER_BOUND('',#911,.T.);
#660=FACE_OUTER_BOUND('',#912,.T.);
#661=FACE_OUTER_BOUND('',#913,.T.);
#662=FACE_OUTER_BOUND('',#914,.T.);
#663=FACE_OUTER_BOUND('',#915,.T.);
#664=FACE_OUTER_BOUND('',#916,.T.);
#665=FACE_OUTER_BOUND('',#917,.T.);
#666=FACE_OUTER_BOUND('',#918,.T.);
#667=FACE_OUTER_BOUND('',#919,.T.);
#668=FACE_OUTER_BOUND('',#920,.T.);
#669=FACE_OUTER_BOUND('',#921,.T.);
#670=FACE_OUTER_BOUND('',#922,.T.);
#671=FACE_OUTER_BOUND('',#923,.T.);
#672=FACE_OUTER_BOUND('',#924,.T.);
#673=FACE_OUTER_BOUND('',#925,.T.);
#674=FACE_OUTER_BOUND('',#926,.T.);
#675=FACE_OUTER_BOUND('',#927,.T.);
#676=FACE_OUTER_BOUND('',#928,.T.);
#677=FACE_OUTER_BOUND('',#929,.T.);
#678=FACE_OUTER_BOUND('',#930,.T.);
#679=FACE_OUTER_BOUND('',#931,.T.);
#680=FACE_OUTER_BOUND('',#932,.T.);
#681=FACE_OUTER_BOUND('',#933,.T.);
#682=FACE_OUTER_BOUND('',#934,.T.);
#683=FACE_OUTER_BOUND('',#935,.T.);
#684=FACE_OUTER_BOUND('',#936,.T.);
#685=FACE_OUTER_BOUND('',#937,.T.);
#686=FACE_OUTER_BOUND('',#939,.T.);
#687=FACE_OUTER_BOUND('',#940,.T.);
#688=FACE_OUTER_BOUND('',#942,.T.);
#689=FACE_OUTER_BOUND('',#943,.T.);
#690=FACE_OUTER_BOUND('',#945,.T.);
#691=FACE_OUTER_BOUND('',#946,.T.);
#692=FACE_OUTER_BOUND('',#948,.T.);
#693=FACE_OUTER_BOUND('',#949,.T.);
#694=FACE_OUTER_BOUND('',#951,.T.);
#695=FACE_OUTER_BOUND('',#952,.T.);
#696=FACE_OUTER_BOUND('',#953,.T.);
#697=FACE_OUTER_BOUND('',#955,.T.);
#698=FACE_OUTER_BOUND('',#956,.T.);
#699=FACE_OUTER_BOUND('',#958,.T.);
#700=FACE_OUTER_BOUND('',#959,.T.);
#701=FACE_OUTER_BOUND('',#961,.T.);
#702=FACE_OUTER_BOUND('',#962,.T.);
#703=FACE_OUTER_BOUND('',#964,.T.);
#704=FACE_OUTER_BOUND('',#965,.T.);
#705=FACE_OUTER_BOUND('',#966,.T.);
#706=FACE_OUTER_BOUND('',#967,.T.);
#707=FACE_OUTER_BOUND('',#968,.T.);
#708=FACE_OUTER_BOUND('',#969,.T.);
#709=FACE_OUTER_BOUND('',#971,.T.);
#710=FACE_OUTER_BOUND('',#972,.T.);
#711=FACE_OUTER_BOUND('',#973,.T.);
#712=FACE_OUTER_BOUND('',#979,.T.);
#713=FACE_OUTER_BOUND('',#985,.T.);
#714=FACE_OUTER_BOUND('',#986,.T.);
#715=FACE_OUTER_BOUND('',#987,.T.);
#716=FACE_OUTER_BOUND('',#988,.T.);
#717=FACE_OUTER_BOUND('',#989,.T.);
#718=FACE_OUTER_BOUND('',#990,.T.);
#719=FACE_OUTER_BOUND('',#991,.T.);
#720=FACE_OUTER_BOUND('',#992,.T.);
#721=FACE_OUTER_BOUND('',#993,.T.);
#722=FACE_OUTER_BOUND('',#994,.T.);
#723=FACE_OUTER_BOUND('',#995,.T.);
#724=FACE_OUTER_BOUND('',#996,.T.);
#725=FACE_OUTER_BOUND('',#997,.T.);
#726=FACE_OUTER_BOUND('',#998,.T.);
#727=FACE_OUTER_BOUND('',#1000,.T.);
#728=FACE_OUTER_BOUND('',#1001,.T.);
#729=FACE_OUTER_BOUND('',#1002,.T.);
#730=FACE_OUTER_BOUND('',#1003,.T.);
#731=FACE_OUTER_BOUND('',#1004,.T.);
#732=FACE_OUTER_BOUND('',#1007,.T.);
#733=FACE_OUTER_BOUND('',#1009,.T.);
#734=FACE_OUTER_BOUND('',#1010,.T.);
#735=FACE_OUTER_BOUND('',#1011,.T.);
#736=FACE_OUTER_BOUND('',#1012,.T.);
#737=FACE_OUTER_BOUND('',#1013,.T.);
#738=FACE_OUTER_BOUND('',#1014,.T.);
#739=FACE_OUTER_BOUND('',#1016,.T.);
#740=FACE_OUTER_BOUND('',#1017,.T.);
#741=FACE_OUTER_BOUND('',#1018,.T.);
#742=FACE_OUTER_BOUND('',#1019,.T.);
#743=FACE_OUTER_BOUND('',#1020,.T.);
#744=FACE_OUTER_BOUND('',#1021,.T.);
#745=FACE_OUTER_BOUND('',#1022,.T.);
#746=FACE_OUTER_BOUND('',#1024,.T.);
#747=FACE_OUTER_BOUND('',#1026,.T.);
#748=FACE_OUTER_BOUND('',#1027,.T.);
#749=FACE_OUTER_BOUND('',#1028,.T.);
#750=FACE_OUTER_BOUND('',#1029,.T.);
#751=FACE_OUTER_BOUND('',#1031,.T.);
#752=FACE_OUTER_BOUND('',#1033,.T.);
#753=FACE_OUTER_BOUND('',#1035,.T.);
#754=FACE_OUTER_BOUND('',#1037,.T.);
#755=FACE_OUTER_BOUND('',#1038,.T.);
#756=FACE_OUTER_BOUND('',#1039,.T.);
#757=FACE_OUTER_BOUND('',#1040,.T.);
#758=FACE_OUTER_BOUND('',#1041,.T.);
#759=FACE_OUTER_BOUND('',#1042,.T.);
#760=FACE_OUTER_BOUND('',#1043,.T.);
#761=FACE_OUTER_BOUND('',#1044,.T.);
#762=FACE_OUTER_BOUND('',#1045,.T.);
#763=FACE_OUTER_BOUND('',#1047,.T.);
#764=FACE_OUTER_BOUND('',#1048,.T.);
#765=EDGE_LOOP('',(#2288,#2289,#2290,#2291));
#766=EDGE_LOOP('',(#2292,#2293,#2294,#2295));
#767=EDGE_LOOP('',(#2296,#2297,#2298,#2299));
#768=EDGE_LOOP('',(#2300,#2301,#2302,#2303));
#769=EDGE_LOOP('',(#2304,#2305,#2306,#2307));
#770=EDGE_LOOP('',(#2308,#2309,#2310,#2311));
#771=EDGE_LOOP('',(#2312,#2313,#2314,#2315));
#772=EDGE_LOOP('',(#2316,#2317,#2318,#2319));
#773=EDGE_LOOP('',(#2320,#2321,#2322,#2323));
#774=EDGE_LOOP('',(#2324,#2325,#2326,#2327));
#775=EDGE_LOOP('',(#2328,#2329,#2330,#2331));
#776=EDGE_LOOP('',(#2332,#2333,#2334,#2335));
#777=EDGE_LOOP('',(#2336,#2337,#2338,#2339));
#778=EDGE_LOOP('',(#2340));
#779=EDGE_LOOP('',(#2341));
#780=EDGE_LOOP('',(#2342));
#781=EDGE_LOOP('',(#2343));
#782=EDGE_LOOP('',(#2344));
#783=EDGE_LOOP('',(#2345));
#784=EDGE_LOOP('',(#2346));
#785=EDGE_LOOP('',(#2347));
#786=EDGE_LOOP('',(#2348,#2349,#2350,#2351));
#787=EDGE_LOOP('',(#2352));
#788=EDGE_LOOP('',(#2353));
#789=EDGE_LOOP('',(#2354));
#790=EDGE_LOOP('',(#2355));
#791=EDGE_LOOP('',(#2356));
#792=EDGE_LOOP('',(#2357));
#793=EDGE_LOOP('',(#2358));
#794=EDGE_LOOP('',(#2359));
#795=EDGE_LOOP('',(#2360,#2361,#2362,#2363,#2364,#2365));
#796=EDGE_LOOP('',(#2366,#2367,#2368,#2369));
#797=EDGE_LOOP('',(#2370));
#798=EDGE_LOOP('',(#2371,#2372,#2373,#2374));
#799=EDGE_LOOP('',(#2375));
#800=EDGE_LOOP('',(#2376,#2377,#2378,#2379));
#801=EDGE_LOOP('',(#2380));
#802=EDGE_LOOP('',(#2381,#2382,#2383,#2384));
#803=EDGE_LOOP('',(#2385));
#804=EDGE_LOOP('',(#2386,#2387));
#805=EDGE_LOOP('',(#2388,#2389,#2390,#2391));
#806=EDGE_LOOP('',(#2392,#2393,#2394,#2395));
#807=EDGE_LOOP('',(#2396,#2397));
#808=EDGE_LOOP('',(#2398,#2399,#2400,#2401));
#809=EDGE_LOOP('',(#2402,#2403));
#810=EDGE_LOOP('',(#2404,#2405,#2406,#2407));
#811=EDGE_LOOP('',(#2408,#2409));
#812=EDGE_LOOP('',(#2410,#2411,#2412,#2413,#2414,#2415,#2416,#2417,#2418,
#2419,#2420,#2421,#2422,#2423,#2424,#2425,#2426,#2427,#2428,#2429));
#813=EDGE_LOOP('',(#2430));
#814=EDGE_LOOP('',(#2431,#2432,#2433,#2434,#2435,#2436,#2437,#2438,#2439));
#815=EDGE_LOOP('',(#2440));
#816=EDGE_LOOP('',(#2441));
#817=EDGE_LOOP('',(#2442));
#818=EDGE_LOOP('',(#2443));
#819=EDGE_LOOP('',(#2444,#2445,#2446,#2447));
#820=EDGE_LOOP('',(#2448,#2449,#2450,#2451));
#821=EDGE_LOOP('',(#2452,#2453,#2454,#2455));
#822=EDGE_LOOP('',(#2456,#2457,#2458,#2459));
#823=EDGE_LOOP('',(#2460,#2461,#2462,#2463));
#824=EDGE_LOOP('',(#2464));
#825=EDGE_LOOP('',(#2465));
#826=EDGE_LOOP('',(#2466,#2467,#2468,#2469));
#827=EDGE_LOOP('',(#2470,#2471));
#828=EDGE_LOOP('',(#2472,#2473,#2474,#2475));
#829=EDGE_LOOP('',(#2476,#2477));
#830=EDGE_LOOP('',(#2478));
#831=EDGE_LOOP('',(#2479));
#832=EDGE_LOOP('',(#2480));
#833=EDGE_LOOP('',(#2481));
#834=EDGE_LOOP('',(#2482));
#835=EDGE_LOOP('',(#2483));
#836=EDGE_LOOP('',(#2484));
#837=EDGE_LOOP('',(#2485));
#838=EDGE_LOOP('',(#2486));
#839=EDGE_LOOP('',(#2487));
#840=EDGE_LOOP('',(#2488));
#841=EDGE_LOOP('',(#2489));
#842=EDGE_LOOP('',(#2490,#2491,#2492,#2493));
#843=EDGE_LOOP('',(#2494,#2495,#2496,#2497));
#844=EDGE_LOOP('',(#2498,#2499,#2500,#2501));
#845=EDGE_LOOP('',(#2502,#2503,#2504,#2505));
#846=EDGE_LOOP('',(#2506,#2507,#2508,#2509));
#847=EDGE_LOOP('',(#2510,#2511,#2512,#2513));
#848=EDGE_LOOP('',(#2514,#2515,#2516,#2517,#2518,#2519));
#849=EDGE_LOOP('',(#2520,#2521,#2522,#2523,#2524,#2525));
#850=EDGE_LOOP('',(#2526));
#851=EDGE_LOOP('',(#2527));
#852=EDGE_LOOP('',(#2528,#2529,#2530,#2531));
#853=EDGE_LOOP('',(#2532,#2533,#2534,#2535));
#854=EDGE_LOOP('',(#2536,#2537,#2538,#2539));
#855=EDGE_LOOP('',(#2540));
#856=EDGE_LOOP('',(#2541));
#857=EDGE_LOOP('',(#2542,#2543,#2544,#2545));
#858=EDGE_LOOP('',(#2546,#2547,#2548,#2549));
#859=EDGE_LOOP('',(#2550,#2551,#2552,#2553));
#860=EDGE_LOOP('',(#2554));
#861=EDGE_LOOP('',(#2555,#2556,#2557,#2558));
#862=EDGE_LOOP('',(#2559));
#863=EDGE_LOOP('',(#2560,#2561,#2562,#2563));
#864=EDGE_LOOP('',(#2564));
#865=EDGE_LOOP('',(#2565,#2566,#2567,#2568));
#866=EDGE_LOOP('',(#2569));
#867=EDGE_LOOP('',(#2570,#2571,#2572,#2573));
#868=EDGE_LOOP('',(#2574));
#869=EDGE_LOOP('',(#2575));
#870=EDGE_LOOP('',(#2576,#2577,#2578,#2579));
#871=EDGE_LOOP('',(#2580,#2581,#2582,#2583));
#872=EDGE_LOOP('',(#2584,#2585,#2586,#2587));
#873=EDGE_LOOP('',(#2588));
#874=EDGE_LOOP('',(#2589));
#875=EDGE_LOOP('',(#2590));
#876=EDGE_LOOP('',(#2591));
#877=EDGE_LOOP('',(#2592));
#878=EDGE_LOOP('',(#2593));
#879=EDGE_LOOP('',(#2594));
#880=EDGE_LOOP('',(#2595));
#881=EDGE_LOOP('',(#2596,#2597,#2598,#2599));
#882=EDGE_LOOP('',(#2600,#2601,#2602,#2603));
#883=EDGE_LOOP('',(#2604,#2605,#2606,#2607));
#884=EDGE_LOOP('',(#2608,#2609,#2610,#2611));
#885=EDGE_LOOP('',(#2612,#2613,#2614,#2615));
#886=EDGE_LOOP('',(#2616));
#887=EDGE_LOOP('',(#2617));
#888=EDGE_LOOP('',(#2618));
#889=EDGE_LOOP('',(#2619,#2620,#2621,#2622));
#890=EDGE_LOOP('',(#2623,#2624,#2625,#2626));
#891=EDGE_LOOP('',(#2627));
#892=EDGE_LOOP('',(#2628,#2629,#2630,#2631,#2632,#2633));
#893=EDGE_LOOP('',(#2634,#2635,#2636,#2637,#2638));
#894=EDGE_LOOP('',(#2639,#2640,#2641,#2642));
#895=EDGE_LOOP('',(#2643,#2644,#2645,#2646));
#896=EDGE_LOOP('',(#2647));
#897=EDGE_LOOP('',(#2648));
#898=EDGE_LOOP('',(#2649,#2650,#2651,#2652,#2653));
#899=EDGE_LOOP('',(#2654));
#900=EDGE_LOOP('',(#2655));
#901=EDGE_LOOP('',(#2656,#2657,#2658,#2659));
#902=EDGE_LOOP('',(#2660,#2661,#2662,#2663,#2664,#2665));
#903=EDGE_LOOP('',(#2666,#2667,#2668,#2669,#2670));
#904=EDGE_LOOP('',(#2671));
#905=EDGE_LOOP('',(#2672));
#906=EDGE_LOOP('',(#2673,#2674,#2675,#2676));
#907=EDGE_LOOP('',(#2677,#2678,#2679,#2680));
#908=EDGE_LOOP('',(#2681,#2682,#2683,#2684));
#909=EDGE_LOOP('',(#2685));
#910=EDGE_LOOP('',(#2686));
#911=EDGE_LOOP('',(#2687,#2688,#2689,#2690,#2691));
#912=EDGE_LOOP('',(#2692,#2693));
#913=EDGE_LOOP('',(#2694,#2695));
#914=EDGE_LOOP('',(#2696,#2697));
#915=EDGE_LOOP('',(#2698,#2699));
#916=EDGE_LOOP('',(#2700,#2701));
#917=EDGE_LOOP('',(#2702,#2703));
#918=EDGE_LOOP('',(#2704,#2705));
#919=EDGE_LOOP('',(#2706,#2707));
#920=EDGE_LOOP('',(#2708,#2709,#2710,#2711));
#921=EDGE_LOOP('',(#2712,#2713,#2714,#2715,#2716,#2717,#2718,#2719,#2720,
#2721,#2722,#2723,#2724,#2725,#2726,#2727,#2728,#2729,#2730,#2731));
#922=EDGE_LOOP('',(#2732,#2733,#2734,#2735));
#923=EDGE_LOOP('',(#2736,#2737,#2738,#2739));
#924=EDGE_LOOP('',(#2740,#2741,#2742,#2743));
#925=EDGE_LOOP('',(#2744,#2745,#2746,#2747));
#926=EDGE_LOOP('',(#2748,#2749,#2750,#2751));
#927=EDGE_LOOP('',(#2752,#2753,#2754,#2755,#2756,#2757));
#928=EDGE_LOOP('',(#2758,#2759,#2760,#2761));
#929=EDGE_LOOP('',(#2762,#2763,#2764,#2765));
#930=EDGE_LOOP('',(#2766,#2767,#2768,#2769));
#931=EDGE_LOOP('',(#2770,#2771,#2772,#2773));
#932=EDGE_LOOP('',(#2774,#2775,#2776,#2777));
#933=EDGE_LOOP('',(#2778,#2779,#2780,#2781));
#934=EDGE_LOOP('',(#2782,#2783,#2784,#2785,#2786,#2787,#2788,#2789,#2790,
#2791,#2792,#2793,#2794,#2795,#2796,#2797,#2798,#2799,#2800,#2801));
#935=EDGE_LOOP('',(#2802,#2803,#2804,#2805));
#936=EDGE_LOOP('',(#2806,#2807,#2808,#2809));
#937=EDGE_LOOP('',(#2810));
#938=EDGE_LOOP('',(#2811));
#939=EDGE_LOOP('',(#2812,#2813,#2814,#2815));
#940=EDGE_LOOP('',(#2816));
#941=EDGE_LOOP('',(#2817));
#942=EDGE_LOOP('',(#2818,#2819,#2820,#2821));
#943=EDGE_LOOP('',(#2822));
#944=EDGE_LOOP('',(#2823));
#945=EDGE_LOOP('',(#2824,#2825,#2826,#2827));
#946=EDGE_LOOP('',(#2828));
#947=EDGE_LOOP('',(#2829));
#948=EDGE_LOOP('',(#2830,#2831,#2832,#2833));
#949=EDGE_LOOP('',(#2834));
#950=EDGE_LOOP('',(#2835));
#951=EDGE_LOOP('',(#2836,#2837,#2838,#2839));
#952=EDGE_LOOP('',(#2840,#2841,#2842,#2843));
#953=EDGE_LOOP('',(#2844));
#954=EDGE_LOOP('',(#2845));
#955=EDGE_LOOP('',(#2846,#2847,#2848,#2849));
#956=EDGE_LOOP('',(#2850));
#957=EDGE_LOOP('',(#2851));
#958=EDGE_LOOP('',(#2852,#2853,#2854,#2855));
#959=EDGE_LOOP('',(#2856));
#960=EDGE_LOOP('',(#2857));
#961=EDGE_LOOP('',(#2858,#2859,#2860,#2861));
#962=EDGE_LOOP('',(#2862));
#963=EDGE_LOOP('',(#2863));
#964=EDGE_LOOP('',(#2864,#2865,#2866,#2867));
#965=EDGE_LOOP('',(#2868,#2869,#2870,#2871));
#966=EDGE_LOOP('',(#2872,#2873,#2874,#2875));
#967=EDGE_LOOP('',(#2876,#2877,#2878,#2879));
#968=EDGE_LOOP('',(#2880,#2881,#2882,#2883));
#969=EDGE_LOOP('',(#2884));
#970=EDGE_LOOP('',(#2885));
#971=EDGE_LOOP('',(#2886,#2887,#2888,#2889));
#972=EDGE_LOOP('',(#2890,#2891,#2892,#2893));
#973=EDGE_LOOP('',(#2894));
#974=EDGE_LOOP('',(#2895));
#975=EDGE_LOOP('',(#2896));
#976=EDGE_LOOP('',(#2897));
#977=EDGE_LOOP('',(#2898));
#978=EDGE_LOOP('',(#2899));
#979=EDGE_LOOP('',(#2900));
#980=EDGE_LOOP('',(#2901));
#981=EDGE_LOOP('',(#2902));
#982=EDGE_LOOP('',(#2903));
#983=EDGE_LOOP('',(#2904));
#984=EDGE_LOOP('',(#2905));
#985=EDGE_LOOP('',(#2906,#2907,#2908,#2909));
#986=EDGE_LOOP('',(#2910,#2911,#2912,#2913));
#987=EDGE_LOOP('',(#2914,#2915,#2916,#2917));
#988=EDGE_LOOP('',(#2918,#2919,#2920,#2921));
#989=EDGE_LOOP('',(#2922,#2923,#2924,#2925));
#990=EDGE_LOOP('',(#2926,#2927,#2928,#2929));
#991=EDGE_LOOP('',(#2930,#2931,#2932,#2933,#2934,#2935));
#992=EDGE_LOOP('',(#2936,#2937,#2938,#2939,#2940,#2941));
#993=EDGE_LOOP('',(#2942));
#994=EDGE_LOOP('',(#2943));
#995=EDGE_LOOP('',(#2944,#2945,#2946,#2947));
#996=EDGE_LOOP('',(#2948,#2949,#2950,#2951));
#997=EDGE_LOOP('',(#2952,#2953,#2954,#2955));
#998=EDGE_LOOP('',(#2956));
#999=EDGE_LOOP('',(#2957));
#1000=EDGE_LOOP('',(#2958,#2959,#2960,#2961));
#1001=EDGE_LOOP('',(#2962,#2963,#2964,#2965));
#1002=EDGE_LOOP('',(#2966,#2967,#2968,#2969));
#1003=EDGE_LOOP('',(#2970,#2971,#2972,#2973));
#1004=EDGE_LOOP('',(#2974,#2975,#2976,#2977));
#1005=EDGE_LOOP('',(#2978));
#1006=EDGE_LOOP('',(#2979));
#1007=EDGE_LOOP('',(#2980));
#1008=EDGE_LOOP('',(#2981));
#1009=EDGE_LOOP('',(#2982,#2983,#2984,#2985));
#1010=EDGE_LOOP('',(#2986,#2987,#2988,#2989));
#1011=EDGE_LOOP('',(#2990));
#1012=EDGE_LOOP('',(#2991,#2992,#2993,#2994));
#1013=EDGE_LOOP('',(#2995,#2996,#2997,#2998));
#1014=EDGE_LOOP('',(#2999));
#1015=EDGE_LOOP('',(#3000));
#1016=EDGE_LOOP('',(#3001,#3002,#3003,#3004));
#1017=EDGE_LOOP('',(#3005,#3006,#3007,#3008));
#1018=EDGE_LOOP('',(#3009,#3010,#3011,#3012));
#1019=EDGE_LOOP('',(#3013));
#1020=EDGE_LOOP('',(#3014,#3015,#3016,#3017));
#1021=EDGE_LOOP('',(#3018,#3019,#3020,#3021));
#1022=EDGE_LOOP('',(#3022));
#1023=EDGE_LOOP('',(#3023));
#1024=EDGE_LOOP('',(#3024));
#1025=EDGE_LOOP('',(#3025));
#1026=EDGE_LOOP('',(#3026,#3027));
#1027=EDGE_LOOP('',(#3028,#3029,#3030,#3031,#3032,#3033,#3034,#3035,#3036));
#1028=EDGE_LOOP('',(#3037,#3038));
#1029=EDGE_LOOP('',(#3039,#3040,#3041,#3042));
#1030=EDGE_LOOP('',(#3043,#3044,#3045,#3046,#3047));
#1031=EDGE_LOOP('',(#3048,#3049,#3050,#3051));
#1032=EDGE_LOOP('',(#3052,#3053));
#1033=EDGE_LOOP('',(#3054));
#1034=EDGE_LOOP('',(#3055));
#1035=EDGE_LOOP('',(#3056));
#1036=EDGE_LOOP('',(#3057));
#1037=EDGE_LOOP('',(#3058));
#1038=EDGE_LOOP('',(#3059,#3060,#3061,#3062));
#1039=EDGE_LOOP('',(#3063,#3064,#3065,#3066));
#1040=EDGE_LOOP('',(#3067,#3068,#3069,#3070));
#1041=EDGE_LOOP('',(#3071,#3072,#3073,#3074));
#1042=EDGE_LOOP('',(#3075,#3076,#3077,#3078));
#1043=EDGE_LOOP('',(#3079,#3080,#3081,#3082));
#1044=EDGE_LOOP('',(#3083,#3084,#3085,#3086,#3087,#3088));
#1045=EDGE_LOOP('',(#3089));
#1046=EDGE_LOOP('',(#3090,#3091,#3092,#3093,#3094,#3095));
#1047=EDGE_LOOP('',(#3096,#3097,#3098,#3099));
#1048=EDGE_LOOP('',(#3100,#3101,#3102,#3103));
#1049=LINE('',#5231,#1219);
#1050=LINE('',#5237,#1220);
#1051=LINE('',#5243,#1221);
#1052=LINE('',#5249,#1222);
#1053=LINE('',#5255,#1223);
#1054=LINE('',#5261,#1224);
#1055=LINE('',#5267,#1225);
#1056=LINE('',#5273,#1226);
#1057=LINE('',#5278,#1227);
#1058=LINE('',#5280,#1228);
#1059=LINE('',#5282,#1229);
#1060=LINE('',#5283,#1230);
#1061=LINE('',#5286,#1231);
#1062=LINE('',#5288,#1232);
#1063=LINE('',#5289,#1233);
#1064=LINE('',#5292,#1234);
#1065=LINE('',#5294,#1235);
#1066=LINE('',#5295,#1236);
#1067=LINE('',#5297,#1237);
#1068=LINE('',#5298,#1238);
#1069=LINE('',#5342,#1239);
#1070=LINE('',#5384,#1240);
#1071=LINE('',#5391,#1241);
#1072=LINE('',#5398,#1242);
#1073=LINE('',#5405,#1243);
#1074=LINE('',#5415,#1244);
#1075=LINE('',#5418,#1245);
#1076=LINE('',#5422,#1246);
#1077=LINE('',#5426,#1247);
#1078=LINE('',#5433,#1248);
#1079=LINE('',#5437,#1249);
#1080=LINE('',#5444,#1250);
#1081=LINE('',#5448,#1251);
#1082=LINE('',#5456,#1252);
#1083=LINE('',#5476,#1253);
#1084=LINE('',#5480,#1254);
#1085=LINE('',#5484,#1255);
#1086=LINE('',#5488,#1256);
#1087=LINE('',#5493,#1257);
#1088=LINE('',#5500,#1258);
#1089=LINE('',#5504,#1259);
#1090=LINE('',#5512,#1260);
#1091=LINE('',#5514,#1261);
#1092=LINE('',#5516,#1262);
#1093=LINE('',#5517,#1263);
#1094=LINE('',#5520,#1264);
#1095=LINE('',#5522,#1265);
#1096=LINE('',#5523,#1266);
#1097=LINE('',#5526,#1267);
#1098=LINE('',#5528,#1268);
#1099=LINE('',#5529,#1269);
#1100=LINE('',#5532,#1270);
#1101=LINE('',#5534,#1271);
#1102=LINE('',#5535,#1272);
#1103=LINE('',#5538,#1273);
#1104=LINE('',#5540,#1274);
#1105=LINE('',#5541,#1275);
#1106=LINE('',#5543,#1276);
#1107=LINE('',#5544,#1277);
#1108=LINE('',#5556,#1278);
#1109=LINE('',#5560,#1279);
#1110=LINE('',#5564,#1280);
#1111=LINE('',#5571,#1281);
#1112=LINE('',#5573,#1282);
#1113=LINE('',#5581,#1283);
#1114=LINE('',#5588,#1284);
#1115=LINE('',#5595,#1285);
#1116=LINE('',#5602,#1286);
#1117=LINE('',#5609,#1287);
#1118=LINE('',#5617,#1288);
#1119=LINE('',#5622,#1289);
#1120=LINE('',#5626,#1290);
#1121=LINE('',#5630,#1291);
#1122=LINE('',#5636,#1292);
#1123=LINE('',#5638,#1293);
#1124=LINE('',#5639,#1294);
#1125=LINE('',#5642,#1295);
#1126=LINE('',#5646,#1296);
#1127=LINE('',#5647,#1297);
#1128=LINE('',#5659,#1298);
#1129=LINE('',#5662,#1299);
#1130=LINE('',#5679,#1300);
#1131=LINE('',#5685,#1301);
#1132=LINE('',#5689,#1302);
#1133=LINE('',#5695,#1303);
#1134=LINE('',#5700,#1304);
#1135=LINE('',#5715,#1305);
#1136=LINE('',#5724,#1306);
#1137=LINE('',#5728,#1307);
#1138=LINE('',#5732,#1308);
#1139=LINE('',#5735,#1309);
#1140=LINE('',#5888,#1310);
#1141=LINE('',#6184,#1311);
#1142=LINE('',#6226,#1312);
#1143=LINE('',#6231,#1313);
#1144=LINE('',#6240,#1314);
#1145=LINE('',#6245,#1315);
#1146=LINE('',#6256,#1316);
#1147=LINE('',#6265,#1317);
#1148=LINE('',#6274,#1318);
#1149=LINE('',#6283,#1319);
#1150=LINE('',#6291,#1320);
#1151=LINE('',#6295,#1321);
#1152=LINE('',#6299,#1322);
#1153=LINE('',#6303,#1323);
#1154=LINE('',#6308,#1324);
#1155=LINE('',#6316,#1325);
#1156=LINE('',#6321,#1326);
#1157=LINE('',#6329,#1327);
#1158=LINE('',#6331,#1328);
#1159=LINE('',#6333,#1329);
#1160=LINE('',#6334,#1330);
#1161=LINE('',#6337,#1331);
#1162=LINE('',#6339,#1332);
#1163=LINE('',#6340,#1333);
#1164=LINE('',#6343,#1334);
#1165=LINE('',#6345,#1335);
#1166=LINE('',#6346,#1336);
#1167=LINE('',#6349,#1337);
#1168=LINE('',#6351,#1338);
#1169=LINE('',#6352,#1339);
#1170=LINE('',#6355,#1340);
#1171=LINE('',#6357,#1341);
#1172=LINE('',#6358,#1342);
#1173=LINE('',#6360,#1343);
#1174=LINE('',#6361,#1344);
#1175=LINE('',#6373,#1345);
#1176=LINE('',#6377,#1346);
#1177=LINE('',#6381,#1347);
#1178=LINE('',#6388,#1348);
#1179=LINE('',#6390,#1349);
#1180=LINE('',#6419,#1350);
#1181=LINE('',#6423,#1351);
#1182=LINE('',#6427,#1352);
#1183=LINE('',#6429,#1353);
#1184=LINE('',#6430,#1354);
#1185=LINE('',#6433,#1355);
#1186=LINE('',#6445,#1356);
#1187=LINE('',#6448,#1357);
#1188=LINE('',#6453,#1358);
#1189=LINE('',#6454,#1359);
#1190=LINE('',#6463,#1360);
#1191=LINE('',#6466,#1361);
#1192=LINE('',#6475,#1362);
#1193=LINE('',#6481,#1363);
#1194=LINE('',#6489,#1364);
#1195=LINE('',#6519,#1365);
#1196=LINE('',#6566,#1366);
#1197=LINE('',#6571,#1367);
#1198=LINE('',#6577,#1368);
#1199=LINE('',#6588,#1369);
#1200=LINE('',#6590,#1370);
#1201=LINE('',#6592,#1371);
#1202=LINE('',#6593,#1372);
#1203=LINE('',#6596,#1373);
#1204=LINE('',#6598,#1374);
#1205=LINE('',#6599,#1375);
#1206=LINE('',#6602,#1376);
#1207=LINE('',#6604,#1377);
#1208=LINE('',#6605,#1378);
#1209=LINE('',#6608,#1379);
#1210=LINE('',#6610,#1380);
#1211=LINE('',#6611,#1381);
#1212=LINE('',#6614,#1382);
#1213=LINE('',#6616,#1383);
#1214=LINE('',#6617,#1384);
#1215=LINE('',#6619,#1385);
#1216=LINE('',#6620,#1386);
#1217=LINE('',#6628,#1387);
#1218=LINE('',#6630,#1388);
#1219=VECTOR('',#4076,0.21);
#1220=VECTOR('',#4083,0.21);
#1221=VECTOR('',#4090,0.210000000000001);
#1222=VECTOR('',#4097,0.210000000000001);
#1223=VECTOR('',#4104,0.21);
#1224=VECTOR('',#4111,0.21);
#1225=VECTOR('',#4118,0.21);
#1226=VECTOR('',#4125,0.21);
#1227=VECTOR('',#4130,1.);
#1228=VECTOR('',#4131,1.);
#1229=VECTOR('',#4132,1.);
#1230=VECTOR('',#4133,1.);
#1231=VECTOR('',#4136,1.);
#1232=VECTOR('',#4137,1.);
#1233=VECTOR('',#4138,1.);
#1234=VECTOR('',#4141,1.);
#1235=VECTOR('',#4142,1.);
#1236=VECTOR('',#4143,1.);
#1237=VECTOR('',#4146,1.);
#1238=VECTOR('',#4147,1.);
#1239=VECTOR('',#4156,0.25);
#1240=VECTOR('',#4161,0.165);
#1241=VECTOR('',#4170,0.165);
#1242=VECTOR('',#4179,0.165);
#1243=VECTOR('',#4188,0.165);
#1244=VECTOR('',#4201,1.);
#1245=VECTOR('',#4204,1.);
#1246=VECTOR('',#4207,1.);
#1247=VECTOR('',#4210,1.);
#1248=VECTOR('',#4219,1.);
#1249=VECTOR('',#4222,1.);
#1250=VECTOR('',#4231,1.);
#1251=VECTOR('',#4234,1.);
#1252=VECTOR('',#4245,2.2);
#1253=VECTOR('',#4272,0.275);
#1254=VECTOR('',#4277,0.275);
#1255=VECTOR('',#4282,0.275);
#1256=VECTOR('',#4287,0.275);
#1257=VECTOR('',#4292,1.5);
#1258=VECTOR('',#4301,3.);
#1259=VECTOR('',#4306,1.02);
#1260=VECTOR('',#4317,1.);
#1261=VECTOR('',#4318,1.);
#1262=VECTOR('',#4319,1.);
#1263=VECTOR('',#4320,1.);
#1264=VECTOR('',#4323,1.);
#1265=VECTOR('',#4324,1.);
#1266=VECTOR('',#4325,1.);
#1267=VECTOR('',#4328,1.);
#1268=VECTOR('',#4329,1.);
#1269=VECTOR('',#4330,1.);
#1270=VECTOR('',#4333,1.);
#1271=VECTOR('',#4334,1.);
#1272=VECTOR('',#4335,1.);
#1273=VECTOR('',#4338,1.);
#1274=VECTOR('',#4339,1.);
#1275=VECTOR('',#4340,1.);
#1276=VECTOR('',#4343,1.);
#1277=VECTOR('',#4344,1.);
#1278=VECTOR('',#4361,0.4);
#1279=VECTOR('',#4366,0.425);
#1280=VECTOR('',#4371,0.41);
#1281=VECTOR('',#4380,0.26);
#1282=VECTOR('',#4383,0.25);
#1283=VECTOR('',#4394,0.165);
#1284=VECTOR('',#4403,0.165);
#1285=VECTOR('',#4412,0.165);
#1286=VECTOR('',#4421,0.165);
#1287=VECTOR('',#4430,1.5);
#1288=VECTOR('',#4441,1.02);
#1289=VECTOR('',#4446,2.2);
#1290=VECTOR('',#4449,1.);
#1291=VECTOR('',#4452,1.);
#1292=VECTOR('',#4461,1.);
#1293=VECTOR('',#4462,1.);
#1294=VECTOR('',#4463,1.);
#1295=VECTOR('',#4466,1.);
#1296=VECTOR('',#4471,1.);
#1297=VECTOR('',#4472,1.);
#1298=VECTOR('',#4489,0.7);
#1299=VECTOR('',#4492,0.5);
#1300=VECTOR('',#4515,0.976185);
#1301=VECTOR('',#4522,0.5);
#1302=VECTOR('',#4527,0.53);
#1303=VECTOR('',#4536,0.976185);
#1304=VECTOR('',#4543,0.53);
#1305=VECTOR('',#4562,1.023815);
#1306=VECTOR('',#4573,1.47);
#1307=VECTOR('',#4578,1.5);
#1308=VECTOR('',#4583,1.47);
#1309=VECTOR('',#4588,1.023815);
#1310=VECTOR('',#4639,1.019052);
#1311=VECTOR('',#4716,0.980948);
#1312=VECTOR('',#4745,1.013815);
#1313=VECTOR('',#4752,0.991185);
#1314=VECTOR('',#4763,1.013815);
#1315=VECTOR('',#4770,0.991185);
#1316=VECTOR('',#4787,0.375);
#1317=VECTOR('',#4798,0.375);
#1318=VECTOR('',#4809,0.375);
#1319=VECTOR('',#4820,0.375);
#1320=VECTOR('',#4831,0.225);
#1321=VECTOR('',#4836,0.225);
#1322=VECTOR('',#4841,0.225);
#1323=VECTOR('',#4846,0.225);
#1324=VECTOR('',#4851,1.49);
#1325=VECTOR('',#4862,0.71);
#1326=VECTOR('',#4867,2.2);
#1327=VECTOR('',#4878,1.);
#1328=VECTOR('',#4879,1.);
#1329=VECTOR('',#4880,1.);
#1330=VECTOR('',#4881,1.);
#1331=VECTOR('',#4884,1.);
#1332=VECTOR('',#4885,1.);
#1333=VECTOR('',#4886,1.);
#1334=VECTOR('',#4889,1.);
#1335=VECTOR('',#4890,1.);
#1336=VECTOR('',#4891,1.);
#1337=VECTOR('',#4894,1.);
#1338=VECTOR('',#4895,1.);
#1339=VECTOR('',#4896,1.);
#1340=VECTOR('',#4899,1.);
#1341=VECTOR('',#4900,1.);
#1342=VECTOR('',#4901,1.);
#1343=VECTOR('',#4904,1.);
#1344=VECTOR('',#4905,1.);
#1345=VECTOR('',#4922,0.325);
#1346=VECTOR('',#4927,0.35);
#1347=VECTOR('',#4932,0.335);
#1348=VECTOR('',#4941,0.21);
#1349=VECTOR('',#4944,0.2);
#1350=VECTOR('',#4997,1.);
#1351=VECTOR('',#5000,1.);
#1352=VECTOR('',#5005,1.);
#1353=VECTOR('',#5006,1.);
#1354=VECTOR('',#5007,1.);
#1355=VECTOR('',#5010,1.);
#1356=VECTOR('',#5025,0.699999999999999);
#1357=VECTOR('',#5028,0.5);
#1358=VECTOR('',#5035,1.);
#1359=VECTOR('',#5036,1.);
#1360=VECTOR('',#5049,0.7);
#1361=VECTOR('',#5052,0.5);
#1362=VECTOR('',#5065,0.505);
#1363=VECTOR('',#5072,0.7);
#1364=VECTOR('',#5083,1.);
#1365=VECTOR('',#5090,0.165);
#1366=VECTOR('',#5093,1.);
#1367=VECTOR('',#5098,0.505);
#1368=VECTOR('',#5105,0.9);
#1369=VECTOR('',#5120,1.);
#1370=VECTOR('',#5121,1.);
#1371=VECTOR('',#5122,1.);
#1372=VECTOR('',#5123,1.);
#1373=VECTOR('',#5126,1.);
#1374=VECTOR('',#5127,1.);
#1375=VECTOR('',#5128,1.);
#1376=VECTOR('',#5131,1.);
#1377=VECTOR('',#5132,1.);
#1378=VECTOR('',#5133,1.);
#1379=VECTOR('',#5136,1.);
#1380=VECTOR('',#5137,1.);
#1381=VECTOR('',#5138,1.);
#1382=VECTOR('',#5141,1.);
#1383=VECTOR('',#5142,1.);
#1384=VECTOR('',#5143,1.);
#1385=VECTOR('',#5146,1.);
#1386=VECTOR('',#5147,1.);
#1387=VECTOR('',#5158,0.185);
#1388=VECTOR('',#5161,0.2);
#1389=CIRCLE('',#3576,0.21);
#1390=CIRCLE('',#3577,0.21);
#1391=CIRCLE('',#3579,0.21);
#1392=CIRCLE('',#3580,0.21);
#1393=CIRCLE('',#3582,0.210000000000001);
#1394=CIRCLE('',#3583,0.210000000000001);
#1395=CIRCLE('',#3585,0.210000000000001);
#1396=CIRCLE('',#3586,0.210000000000001);
#1397=CIRCLE('',#3588,0.21);
#1398=CIRCLE('',#3589,0.21);
#1399=CIRCLE('',#3591,0.21);
#1400=CIRCLE('',#3592,0.21);
#1401=CIRCLE('',#3594,0.21);
#1402=CIRCLE('',#3595,0.21);
#1403=CIRCLE('',#3597,0.21);
#1404=CIRCLE('',#3598,0.21);
#1405=CIRCLE('',#3608,0.165);
#1406=CIRCLE('',#3609,0.165);
#1407=CIRCLE('',#3612,0.165);
#1408=CIRCLE('',#3613,0.165);
#1409=CIRCLE('',#3616,0.165);
#1410=CIRCLE('',#3617,0.165);
#1411=CIRCLE('',#3620,0.165);
#1412=CIRCLE('',#3621,0.165);
#1413=CIRCLE('',#3624,2.2);
#1414=CIRCLE('',#3625,0.525);
#1415=CIRCLE('',#3627,0.525);
#1416=CIRCLE('',#3629,0.525);
#1417=CIRCLE('',#3630,0.525);
#1418=CIRCLE('',#3632,2.2);
#1419=CIRCLE('',#3634,0.525);
#1420=CIRCLE('',#3635,0.525);
#1421=CIRCLE('',#3637,2.2);
#1422=CIRCLE('',#3639,0.525);
#1423=CIRCLE('',#3640,0.525);
#1424=CIRCLE('',#3642,2.2);
#1425=CIRCLE('',#3644,2.2);
#1426=CIRCLE('',#3645,2.2);
#1427=CIRCLE('',#3646,2.2);
#1428=CIRCLE('',#3647,2.2);
#1429=CIRCLE('',#3648,2.2);
#1430=CIRCLE('',#3649,2.2);
#1431=CIRCLE('',#3651,3.);
#1432=CIRCLE('',#3652,0.275);
#1433=CIRCLE('',#3653,0.275);
#1434=CIRCLE('',#3654,0.275);
#1435=CIRCLE('',#3655,0.275);
#1436=CIRCLE('',#3657,0.275);
#1437=CIRCLE('',#3659,0.275);
#1438=CIRCLE('',#3661,0.275);
#1439=CIRCLE('',#3663,0.275);
#1440=CIRCLE('',#3665,1.5);
#1441=CIRCLE('',#3666,1.5);
#1442=CIRCLE('',#3668,1.02);
#1443=CIRCLE('',#3670,3.);
#1444=CIRCLE('',#3672,1.02);
#1445=CIRCLE('',#3685,0.24505);
#1446=CIRCLE('',#3687,0.375);
#1447=CIRCLE('',#3689,0.425);
#1448=CIRCLE('',#3691,0.425);
#1449=CIRCLE('',#3693,0.395);
#1450=CIRCLE('',#3695,0.27);
#1451=CIRCLE('',#3697,0.24505);
#1452=CIRCLE('',#3703,0.165);
#1453=CIRCLE('',#3704,0.165);
#1454=CIRCLE('',#3707,0.165);
#1455=CIRCLE('',#3708,0.165);
#1456=CIRCLE('',#3711,0.165);
#1457=CIRCLE('',#3712,0.165);
#1458=CIRCLE('',#3715,0.165);
#1459=CIRCLE('',#3716,0.165);
#1460=CIRCLE('',#3719,1.5);
#1461=CIRCLE('',#3720,1.5);
#1462=CIRCLE('',#3722,1.02);
#1463=CIRCLE('',#3724,1.02);
#1464=CIRCLE('',#3726,2.2);
#1465=CIRCLE('',#3727,2.2);
#1466=CIRCLE('',#3728,2.2);
#1467=CIRCLE('',#3729,2.2);
#1468=CIRCLE('',#3734,1.);
#1469=CIRCLE('',#3737,1.);
#1470=CIRCLE('',#3739,0.7);
#1471=CIRCLE('',#3741,0.7);
#1472=CIRCLE('',#3742,0.5);
#1473=CIRCLE('',#3745,0.5);
#1474=CIRCLE('',#3750,0.976185);
#1475=CIRCLE('',#3751,0.976185);
#1476=CIRCLE('',#3752,0.247676);
#1477=CIRCLE('',#3753,0.976185);
#1478=CIRCLE('',#3754,0.976185);
#1479=CIRCLE('',#3756,0.976185);
#1480=CIRCLE('',#3758,0.5);
#1481=CIRCLE('',#3759,0.5);
#1482=CIRCLE('',#3761,0.56);
#1483=CIRCLE('',#3764,0.976185);
#1484=CIRCLE('',#3766,0.56);
#1485=CIRCLE('',#3770,1.023815);
#1486=CIRCLE('',#3771,1.023815);
#1487=CIRCLE('',#3772,0.247676);
#1488=CIRCLE('',#3773,1.023815);
#1489=CIRCLE('',#3774,1.023815);
#1490=CIRCLE('',#3776,1.023815);
#1491=CIRCLE('',#3778,1.44);
#1492=CIRCLE('',#3779,1.023815);
#1493=CIRCLE('',#3781,1.5);
#1494=CIRCLE('',#3783,1.5);
#1495=CIRCLE('',#3785,1.44);
#1496=CIRCLE('',#3790,0.23815);
#1497=CIRCLE('',#3792,0.23815);
#1498=CIRCLE('',#3794,0.23815);
#1499=CIRCLE('',#3796,0.23815);
#1500=CIRCLE('',#3798,0.23815);
#1501=CIRCLE('',#3800,0.23815);
#1502=CIRCLE('',#3802,0.23815);
#1503=CIRCLE('',#3804,0.23815);
#1504=CIRCLE('',#3807,0.243053047864041);
#1505=CIRCLE('',#3808,0.243053047864041);
#1506=CIRCLE('',#3810,1.019052);
#1507=CIRCLE('',#3811,1.019052);
#1508=CIRCLE('',#3812,1.019052);
#1509=CIRCLE('',#3813,1.019052);
#1510=CIRCLE('',#3814,1.019052);
#1511=CIRCLE('',#3815,1.019052);
#1512=CIRCLE('',#3816,1.019052);
#1513=CIRCLE('',#3817,1.019052);
#1514=CIRCLE('',#3818,1.019052);
#1515=CIRCLE('',#3820,0.980948);
#1516=CIRCLE('',#3821,0.243053047864041);
#1517=CIRCLE('',#3823,0.243053047864041);
#1518=CIRCLE('',#3825,0.980948);
#1519=CIRCLE('',#3826,0.243053047864041);
#1520=CIRCLE('',#3828,0.243053047864041);
#1521=CIRCLE('',#3830,0.980948);
#1522=CIRCLE('',#3831,0.243053047864041);
#1523=CIRCLE('',#3833,0.243053047864041);
#1524=CIRCLE('',#3835,0.980948);
#1525=CIRCLE('',#3836,0.243053047864041);
#1526=CIRCLE('',#3838,0.243053047864041);
#1527=CIRCLE('',#3840,0.980948);
#1528=CIRCLE('',#3841,0.243053047864041);
#1529=CIRCLE('',#3843,0.243053047864041);
#1530=CIRCLE('',#3845,0.980948);
#1531=CIRCLE('',#3846,0.243053047864041);
#1532=CIRCLE('',#3848,0.243053047864041);
#1533=CIRCLE('',#3850,0.980948);
#1534=CIRCLE('',#3851,0.980948);
#1535=CIRCLE('',#3852,0.980948);
#1536=CIRCLE('',#3854,0.243053047864041);
#1537=CIRCLE('',#3856,0.243053047864041);
#1538=CIRCLE('',#3861,1.013815);
#1539=CIRCLE('',#3862,0.991185);
#1540=CIRCLE('',#3864,1.013815);
#1541=CIRCLE('',#3866,0.991185);
#1542=CIRCLE('',#3869,1.013815);
#1543=CIRCLE('',#3870,0.991185);
#1544=CIRCLE('',#3872,1.013815);
#1545=CIRCLE('',#3874,0.991185);
#1546=CIRCLE('',#3883,0.375);
#1547=CIRCLE('',#3884,0.375);
#1548=CIRCLE('',#3886,0.225);
#1549=CIRCLE('',#3888,0.375);
#1550=CIRCLE('',#3889,0.375);
#1551=CIRCLE('',#3891,0.225);
#1552=CIRCLE('',#3893,0.375);
#1553=CIRCLE('',#3894,0.375);
#1554=CIRCLE('',#3896,0.225);
#1555=CIRCLE('',#3898,0.375);
#1556=CIRCLE('',#3899,0.375);
#1557=CIRCLE('',#3901,0.225);
#1558=CIRCLE('',#3903,0.225);
#1559=CIRCLE('',#3905,0.225);
#1560=CIRCLE('',#3907,0.225);
#1561=CIRCLE('',#3909,0.225);
#1562=CIRCLE('',#3911,1.49);
#1563=CIRCLE('',#3912,1.49);
#1564=CIRCLE('',#3914,0.71);
#1565=CIRCLE('',#3916,0.71);
#1566=CIRCLE('',#3918,2.2);
#1567=CIRCLE('',#3919,2.2);
#1568=CIRCLE('',#3932,0.1954);
#1569=CIRCLE('',#3934,0.3);
#1570=CIRCLE('',#3936,0.35);
#1571=CIRCLE('',#3938,0.35);
#1572=CIRCLE('',#3940,0.32);
#1573=CIRCLE('',#3942,0.22);
#1574=CIRCLE('',#3944,0.1954);
#1575=CIRCLE('',#3972,1.);
#1576=CIRCLE('',#3973,1.);
#1577=CIRCLE('',#3976,1.);
#1578=CIRCLE('',#3977,0.699999999999999);
#1579=CIRCLE('',#3978,0.7);
#1580=CIRCLE('',#3980,0.699999999999999);
#1581=CIRCLE('',#3981,0.5);
#1582=CIRCLE('',#3984,0.5);
#1583=CIRCLE('',#3988,1.);
#1584=CIRCLE('',#3990,0.7);
#1585=CIRCLE('',#3991,0.5);
#1586=CIRCLE('',#3994,0.5);
#1587=CIRCLE('',#3999,0.505);
#1588=CIRCLE('',#4000,0.505);
#1589=CIRCLE('',#4002,0.7);
#1590=CIRCLE('',#4003,0.7);
#1591=CIRCLE('',#4008,0.165);
#1592=CIRCLE('',#4010,0.165);
#1593=CIRCLE('',#4013,0.505);
#1594=CIRCLE('',#4014,0.505);
#1595=CIRCLE('',#4016,0.9);
#1596=CIRCLE('',#4017,0.9);
#1597=CIRCLE('',#4022,0.1954);
#1598=CIRCLE('',#4031,0.17);
#1599=CIRCLE('',#4033,0.1954);
#1600=VERTEX_POINT('',#5228);
#1601=VERTEX_POINT('',#5230);
#1602=VERTEX_POINT('',#5234);
#1603=VERTEX_POINT('',#5236);
#1604=VERTEX_POINT('',#5240);
#1605=VERTEX_POINT('',#5242);
#1606=VERTEX_POINT('',#5246);
#1607=VERTEX_POINT('',#5248);
#1608=VERTEX_POINT('',#5252);
#1609=VERTEX_POINT('',#5254);
#1610=VERTEX_POINT('',#5258);
#1611=VERTEX_POINT('',#5260);
#1612=VERTEX_POINT('',#5264);
#1613=VERTEX_POINT('',#5266);
#1614=VERTEX_POINT('',#5270);
#1615=VERTEX_POINT('',#5272);
#1616=VERTEX_POINT('',#5276);
#1617=VERTEX_POINT('',#5277);
#1618=VERTEX_POINT('',#5279);
#1619=VERTEX_POINT('',#5281);
#1620=VERTEX_POINT('',#5285);
#1621=VERTEX_POINT('',#5287);
#1622=VERTEX_POINT('',#5291);
#1623=VERTEX_POINT('',#5293);
#1624=VERTEX_POINT('',#5303);
#1625=VERTEX_POINT('',#5304);
#1626=VERTEX_POINT('',#5341);
#1627=VERTEX_POINT('',#5343);
#1628=VERTEX_POINT('',#5381);
#1629=VERTEX_POINT('',#5383);
#1630=VERTEX_POINT('',#5388);
#1631=VERTEX_POINT('',#5390);
#1632=VERTEX_POINT('',#5395);
#1633=VERTEX_POINT('',#5397);
#1634=VERTEX_POINT('',#5402);
#1635=VERTEX_POINT('',#5404);
#1636=VERTEX_POINT('',#5409);
#1637=VERTEX_POINT('',#5410);
#1638=VERTEX_POINT('',#5414);
#1639=VERTEX_POINT('',#5416);
#1640=VERTEX_POINT('',#5420);
#1641=VERTEX_POINT('',#5421);
#1642=VERTEX_POINT('',#5423);
#1643=VERTEX_POINT('',#5425);
#1644=VERTEX_POINT('',#5431);
#1645=VERTEX_POINT('',#5432);
#1646=VERTEX_POINT('',#5434);
#1647=VERTEX_POINT('',#5436);
#1648=VERTEX_POINT('',#5442);
#1649=VERTEX_POINT('',#5443);
#1650=VERTEX_POINT('',#5445);
#1651=VERTEX_POINT('',#5447);
#1652=VERTEX_POINT('',#5453);
#1653=VERTEX_POINT('',#5455);
#1654=VERTEX_POINT('',#5463);
#1655=VERTEX_POINT('',#5465);
#1656=VERTEX_POINT('',#5467);
#1657=VERTEX_POINT('',#5469);
#1658=VERTEX_POINT('',#5471);
#1659=VERTEX_POINT('',#5474);
#1660=VERTEX_POINT('',#5478);
#1661=VERTEX_POINT('',#5482);
#1662=VERTEX_POINT('',#5486);
#1663=VERTEX_POINT('',#5490);
#1664=VERTEX_POINT('',#5492);
#1665=VERTEX_POINT('',#5496);
#1666=VERTEX_POINT('',#5499);
#1667=VERTEX_POINT('',#5503);
#1668=VERTEX_POINT('',#5510);
#1669=VERTEX_POINT('',#5511);
#1670=VERTEX_POINT('',#5513);
#1671=VERTEX_POINT('',#5515);
#1672=VERTEX_POINT('',#5519);
#1673=VERTEX_POINT('',#5521);
#1674=VERTEX_POINT('',#5525);
#1675=VERTEX_POINT('',#5527);
#1676=VERTEX_POINT('',#5531);
#1677=VERTEX_POINT('',#5533);
#1678=VERTEX_POINT('',#5537);
#1679=VERTEX_POINT('',#5539);
#1680=VERTEX_POINT('',#5548);
#1681=VERTEX_POINT('',#5551);
#1682=VERTEX_POINT('',#5554);
#1683=VERTEX_POINT('',#5558);
#1684=VERTEX_POINT('',#5562);
#1685=VERTEX_POINT('',#5566);
#1686=VERTEX_POINT('',#5569);
#1687=VERTEX_POINT('',#5578);
#1688=VERTEX_POINT('',#5580);
#1689=VERTEX_POINT('',#5585);
#1690=VERTEX_POINT('',#5587);
#1691=VERTEX_POINT('',#5592);
#1692=VERTEX_POINT('',#5594);
#1693=VERTEX_POINT('',#5599);
#1694=VERTEX_POINT('',#5601);
#1695=VERTEX_POINT('',#5606);
#1696=VERTEX_POINT('',#5608);
#1697=VERTEX_POINT('',#5612);
#1698=VERTEX_POINT('',#5615);
#1699=VERTEX_POINT('',#5619);
#1700=VERTEX_POINT('',#5621);
#1701=VERTEX_POINT('',#5624);
#1702=VERTEX_POINT('',#5625);
#1703=VERTEX_POINT('',#5627);
#1704=VERTEX_POINT('',#5629);
#1705=VERTEX_POINT('',#5635);
#1706=VERTEX_POINT('',#5637);
#1707=VERTEX_POINT('',#5641);
#1708=VERTEX_POINT('',#5645);
#1709=VERTEX_POINT('',#5651);
#1710=VERTEX_POINT('',#5654);
#1711=VERTEX_POINT('',#5656);
#1712=VERTEX_POINT('',#5661);
#1713=VERTEX_POINT('',#5668);
#1714=VERTEX_POINT('',#5669);
#1715=VERTEX_POINT('',#5672);
#1716=VERTEX_POINT('',#5674);
#1717=VERTEX_POINT('',#5678);
#1718=VERTEX_POINT('',#5682);
#1719=VERTEX_POINT('',#5684);
#1720=VERTEX_POINT('',#5688);
#1721=VERTEX_POINT('',#5693);
#1722=VERTEX_POINT('',#5697);
#1723=VERTEX_POINT('',#5703);
#1724=VERTEX_POINT('',#5704);
#1725=VERTEX_POINT('',#5707);
#1726=VERTEX_POINT('',#5709);
#1727=VERTEX_POINT('',#5713);
#1728=VERTEX_POINT('',#5717);
#1729=VERTEX_POINT('',#5719);
#1730=VERTEX_POINT('',#5722);
#1731=VERTEX_POINT('',#5726);
#1732=VERTEX_POINT('',#5730);
#1733=VERTEX_POINT('',#5738);
#1734=VERTEX_POINT('',#5739);
#1735=VERTEX_POINT('',#5742);
#1736=VERTEX_POINT('',#5743);
#1737=VERTEX_POINT('',#5746);
#1738=VERTEX_POINT('',#5747);
#1739=VERTEX_POINT('',#5750);
#1740=VERTEX_POINT('',#5751);
#1741=VERTEX_POINT('',#5754);
#1742=VERTEX_POINT('',#5755);
#1743=VERTEX_POINT('',#5758);
#1744=VERTEX_POINT('',#5759);
#1745=VERTEX_POINT('',#5762);
#1746=VERTEX_POINT('',#5763);
#1747=VERTEX_POINT('',#5766);
#1748=VERTEX_POINT('',#5767);
#1749=VERTEX_POINT('',#5771);
#1750=VERTEX_POINT('',#5772);
#1751=VERTEX_POINT('',#5795);
#1752=VERTEX_POINT('',#5797);
#1753=VERTEX_POINT('',#5822);
#1754=VERTEX_POINT('',#5824);
#1755=VERTEX_POINT('',#5847);
#1756=VERTEX_POINT('',#5849);
#1757=VERTEX_POINT('',#5872);
#1758=VERTEX_POINT('',#5874);
#1759=VERTEX_POINT('',#5887);
#1760=VERTEX_POINT('',#5890);
#1761=VERTEX_POINT('',#5903);
#1762=VERTEX_POINT('',#5905);
#1763=VERTEX_POINT('',#5928);
#1764=VERTEX_POINT('',#5930);
#1765=VERTEX_POINT('',#5953);
#1766=VERTEX_POINT('',#5955);
#1767=VERTEX_POINT('',#5978);
#1768=VERTEX_POINT('',#5980);
#1769=VERTEX_POINT('',#6005);
#1770=VERTEX_POINT('',#6009);
#1771=VERTEX_POINT('',#6034);
#1772=VERTEX_POINT('',#6038);
#1773=VERTEX_POINT('',#6063);
#1774=VERTEX_POINT('',#6067);
#1775=VERTEX_POINT('',#6068);
#1776=VERTEX_POINT('',#6095);
#1777=VERTEX_POINT('',#6099);
#1778=VERTEX_POINT('',#6124);
#1779=VERTEX_POINT('',#6128);
#1780=VERTEX_POINT('',#6153);
#1781=VERTEX_POINT('',#6157);
#1782=VERTEX_POINT('',#6182);
#1783=VERTEX_POINT('',#6185);
#1784=VERTEX_POINT('',#6187);
#1785=VERTEX_POINT('',#6219);
#1786=VERTEX_POINT('',#6221);
#1787=VERTEX_POINT('',#6224);
#1788=VERTEX_POINT('',#6228);
#1789=VERTEX_POINT('',#6233);
#1790=VERTEX_POINT('',#6235);
#1791=VERTEX_POINT('',#6238);
#1792=VERTEX_POINT('',#6242);
#1793=VERTEX_POINT('',#6253);
#1794=VERTEX_POINT('',#6255);
#1795=VERTEX_POINT('',#6259);
#1796=VERTEX_POINT('',#6262);
#1797=VERTEX_POINT('',#6264);
#1798=VERTEX_POINT('',#6268);
#1799=VERTEX_POINT('',#6271);
#1800=VERTEX_POINT('',#6273);
#1801=VERTEX_POINT('',#6277);
#1802=VERTEX_POINT('',#6280);
#1803=VERTEX_POINT('',#6282);
#1804=VERTEX_POINT('',#6286);
#1805=VERTEX_POINT('',#6289);
#1806=VERTEX_POINT('',#6293);
#1807=VERTEX_POINT('',#6297);
#1808=VERTEX_POINT('',#6301);
#1809=VERTEX_POINT('',#6305);
#1810=VERTEX_POINT('',#6307);
#1811=VERTEX_POINT('',#6311);
#1812=VERTEX_POINT('',#6314);
#1813=VERTEX_POINT('',#6318);
#1814=VERTEX_POINT('',#6320);
#1815=VERTEX_POINT('',#6327);
#1816=VERTEX_POINT('',#6328);
#1817=VERTEX_POINT('',#6330);
#1818=VERTEX_POINT('',#6332);
#1819=VERTEX_POINT('',#6336);
#1820=VERTEX_POINT('',#6338);
#1821=VERTEX_POINT('',#6342);
#1822=VERTEX_POINT('',#6344);
#1823=VERTEX_POINT('',#6348);
#1824=VERTEX_POINT('',#6350);
#1825=VERTEX_POINT('',#6354);
#1826=VERTEX_POINT('',#6356);
#1827=VERTEX_POINT('',#6365);
#1828=VERTEX_POINT('',#6368);
#1829=VERTEX_POINT('',#6371);
#1830=VERTEX_POINT('',#6375);
#1831=VERTEX_POINT('',#6379);
#1832=VERTEX_POINT('',#6383);
#1833=VERTEX_POINT('',#6386);
#1834=VERTEX_POINT('',#6417);
#1835=VERTEX_POINT('',#6418);
#1836=VERTEX_POINT('',#6420);
#1837=VERTEX_POINT('',#6422);
#1838=VERTEX_POINT('',#6426);
#1839=VERTEX_POINT('',#6428);
#1840=VERTEX_POINT('',#6432);
#1841=VERTEX_POINT('',#6435);
#1842=VERTEX_POINT('',#6437);
#1843=VERTEX_POINT('',#6440);
#1844=VERTEX_POINT('',#6442);
#1845=VERTEX_POINT('',#6447);
#1846=VERTEX_POINT('',#6452);
#1847=VERTEX_POINT('',#6458);
#1848=VERTEX_POINT('',#6460);
#1849=VERTEX_POINT('',#6465);
#1850=VERTEX_POINT('',#6472);
#1851=VERTEX_POINT('',#6474);
#1852=VERTEX_POINT('',#6478);
#1853=VERTEX_POINT('',#6480);
#1854=VERTEX_POINT('',#6487);
#1855=VERTEX_POINT('',#6488);
#1856=VERTEX_POINT('',#6492);
#1857=VERTEX_POINT('',#6507);
#1858=VERTEX_POINT('',#6509);
#1859=VERTEX_POINT('',#6518);
#1860=VERTEX_POINT('',#6520);
#1861=VERTEX_POINT('',#6568);
#1862=VERTEX_POINT('',#6570);
#1863=VERTEX_POINT('',#6574);
#1864=VERTEX_POINT('',#6576);
#1865=VERTEX_POINT('',#6583);
#1866=VERTEX_POINT('',#6586);
#1867=VERTEX_POINT('',#6587);
#1868=VERTEX_POINT('',#6589);
#1869=VERTEX_POINT('',#6591);
#1870=VERTEX_POINT('',#6595);
#1871=VERTEX_POINT('',#6597);
#1872=VERTEX_POINT('',#6601);
#1873=VERTEX_POINT('',#6603);
#1874=VERTEX_POINT('',#6607);
#1875=VERTEX_POINT('',#6609);
#1876=VERTEX_POINT('',#6613);
#1877=VERTEX_POINT('',#6615);
#1878=VERTEX_POINT('',#6623);
#1879=VERTEX_POINT('',#6626);
#1880=EDGE_CURVE('',#1600,#1600,#1389,.T.);
#1881=EDGE_CURVE('',#1600,#1601,#1049,.T.);
#1882=EDGE_CURVE('',#1601,#1601,#1390,.T.);
#1883=EDGE_CURVE('',#1602,#1602,#1391,.T.);
#1884=EDGE_CURVE('',#1602,#1603,#1050,.T.);
#1885=EDGE_CURVE('',#1603,#1603,#1392,.T.);
#1886=EDGE_CURVE('',#1604,#1604,#1393,.T.);
#1887=EDGE_CURVE('',#1604,#1605,#1051,.T.);
#1888=EDGE_CURVE('',#1605,#1605,#1394,.T.);
#1889=EDGE_CURVE('',#1606,#1606,#1395,.T.);
#1890=EDGE_CURVE('',#1606,#1607,#1052,.T.);
#1891=EDGE_CURVE('',#1607,#1607,#1396,.T.);
#1892=EDGE_CURVE('',#1608,#1608,#1397,.T.);
#1893=EDGE_CURVE('',#1608,#1609,#1053,.T.);
#1894=EDGE_CURVE('',#1609,#1609,#1398,.T.);
#1895=EDGE_CURVE('',#1610,#1610,#1399,.T.);
#1896=EDGE_CURVE('',#1610,#1611,#1054,.T.);
#1897=EDGE_CURVE('',#1611,#1611,#1400,.T.);
#1898=EDGE_CURVE('',#1612,#1612,#1401,.T.);
#1899=EDGE_CURVE('',#1612,#1613,#1055,.T.);
#1900=EDGE_CURVE('',#1613,#1613,#1402,.T.);
#1901=EDGE_CURVE('',#1614,#1614,#1403,.T.);
#1902=EDGE_CURVE('',#1614,#1615,#1056,.T.);
#1903=EDGE_CURVE('',#1615,#1615,#1404,.T.);
#1904=EDGE_CURVE('',#1616,#1617,#1057,.T.);
#1905=EDGE_CURVE('',#1617,#1618,#1058,.T.);
#1906=EDGE_CURVE('',#1619,#1618,#1059,.T.);
#1907=EDGE_CURVE('',#1616,#1619,#1060,.T.);
#1908=EDGE_CURVE('',#1620,#1616,#1061,.T.);
#1909=EDGE_CURVE('',#1621,#1619,#1062,.T.);
#1910=EDGE_CURVE('',#1620,#1621,#1063,.T.);
#1911=EDGE_CURVE('',#1622,#1620,#1064,.T.);
#1912=EDGE_CURVE('',#1623,#1621,#1065,.T.);
#1913=EDGE_CURVE('',#1622,#1623,#1066,.T.);
#1914=EDGE_CURVE('',#1617,#1622,#1067,.T.);
#1915=EDGE_CURVE('',#1618,#1623,#1068,.T.);
#1916=EDGE_CURVE('',#1624,#1625,#280,.T.);
#1917=EDGE_CURVE('',#1625,#1624,#281,.T.);
#1918=EDGE_CURVE('',#1625,#1626,#1069,.T.);
#1919=EDGE_CURVE('',#1627,#1626,#282,.T.);
#1920=EDGE_CURVE('',#1626,#1627,#283,.T.);
#1921=EDGE_CURVE('',#1628,#1628,#1405,.T.);
#1922=EDGE_CURVE('',#1628,#1629,#1070,.T.);
#1923=EDGE_CURVE('',#1629,#1629,#1406,.T.);
#1924=EDGE_CURVE('',#1630,#1630,#1407,.T.);
#1925=EDGE_CURVE('',#1630,#1631,#1071,.T.);
#1926=EDGE_CURVE('',#1631,#1631,#1408,.T.);
#1927=EDGE_CURVE('',#1632,#1632,#1409,.T.);
#1928=EDGE_CURVE('',#1632,#1633,#1072,.T.);
#1929=EDGE_CURVE('',#1633,#1633,#1410,.T.);
#1930=EDGE_CURVE('',#1634,#1634,#1411,.T.);
#1931=EDGE_CURVE('',#1634,#1635,#1073,.T.);
#1932=EDGE_CURVE('',#1635,#1635,#1412,.T.);
#1933=EDGE_CURVE('',#1636,#1637,#1413,.T.);
#1934=EDGE_CURVE('',#1637,#1636,#1414,.T.);
#1935=EDGE_CURVE('',#1638,#1636,#1074,.T.);
#1936=EDGE_CURVE('',#1639,#1638,#1415,.T.);
#1937=EDGE_CURVE('',#1637,#1639,#1075,.T.);
#1938=EDGE_CURVE('',#1640,#1641,#1076,.T.);
#1939=EDGE_CURVE('',#1640,#1642,#1416,.T.);
#1940=EDGE_CURVE('',#1643,#1642,#1077,.T.);
#1941=EDGE_CURVE('',#1641,#1643,#1417,.T.);
#1942=EDGE_CURVE('',#1642,#1640,#1418,.T.);
#1943=EDGE_CURVE('',#1644,#1645,#1078,.T.);
#1944=EDGE_CURVE('',#1644,#1646,#1419,.T.);
#1945=EDGE_CURVE('',#1647,#1646,#1079,.T.);
#1946=EDGE_CURVE('',#1645,#1647,#1420,.T.);
#1947=EDGE_CURVE('',#1646,#1644,#1421,.T.);
#1948=EDGE_CURVE('',#1648,#1649,#1080,.T.);
#1949=EDGE_CURVE('',#1648,#1650,#1422,.T.);
#1950=EDGE_CURVE('',#1651,#1650,#1081,.T.);
#1951=EDGE_CURVE('',#1649,#1651,#1423,.T.);
#1952=EDGE_CURVE('',#1650,#1648,#1424,.T.);
#1953=EDGE_CURVE('',#1652,#1652,#1425,.T.);
#1954=EDGE_CURVE('',#1652,#1653,#1082,.T.);
#1955=EDGE_CURVE('',#1653,#1638,#1426,.T.);
#1956=EDGE_CURVE('',#1639,#1651,#1427,.T.);
#1957=EDGE_CURVE('',#1649,#1647,#1428,.T.);
#1958=EDGE_CURVE('',#1645,#1643,#1429,.T.);
#1959=EDGE_CURVE('',#1641,#1653,#1430,.T.);
#1960=EDGE_CURVE('',#1654,#1654,#1431,.T.);
#1961=EDGE_CURVE('',#1655,#1655,#1432,.T.);
#1962=EDGE_CURVE('',#1656,#1656,#1433,.T.);
#1963=EDGE_CURVE('',#1657,#1657,#1434,.T.);
#1964=EDGE_CURVE('',#1658,#1658,#1435,.T.);
#1965=EDGE_CURVE('',#1659,#1659,#1436,.T.);
#1966=EDGE_CURVE('',#1659,#1655,#1083,.T.);
#1967=EDGE_CURVE('',#1660,#1660,#1437,.T.);
#1968=EDGE_CURVE('',#1660,#1658,#1084,.T.);
#1969=EDGE_CURVE('',#1661,#1661,#1438,.T.);
#1970=EDGE_CURVE('',#1661,#1656,#1085,.T.);
#1971=EDGE_CURVE('',#1662,#1662,#1439,.T.);
#1972=EDGE_CURVE('',#1662,#1657,#1086,.T.);
#1973=EDGE_CURVE('',#1663,#1663,#1440,.T.);
#1974=EDGE_CURVE('',#1663,#1664,#1087,.T.);
#1975=EDGE_CURVE('',#1664,#1664,#1441,.T.);
#1976=EDGE_CURVE('',#1665,#1665,#1442,.T.);
#1977=EDGE_CURVE('',#1654,#1666,#1088,.T.);
#1978=EDGE_CURVE('',#1666,#1666,#1443,.T.);
#1979=EDGE_CURVE('',#1665,#1667,#1089,.T.);
#1980=EDGE_CURVE('',#1667,#1667,#1444,.T.);
#1981=EDGE_CURVE('',#1668,#1669,#1090,.T.);
#1982=EDGE_CURVE('',#1669,#1670,#1091,.T.);
#1983=EDGE_CURVE('',#1670,#1671,#1092,.T.);
#1984=EDGE_CURVE('',#1668,#1671,#1093,.T.);
#1985=EDGE_CURVE('',#1669,#1672,#1094,.T.);
#1986=EDGE_CURVE('',#1672,#1673,#1095,.T.);
#1987=EDGE_CURVE('',#1673,#1670,#1096,.T.);
#1988=EDGE_CURVE('',#1672,#1674,#1097,.T.);
#1989=EDGE_CURVE('',#1674,#1675,#1098,.T.);
#1990=EDGE_CURVE('',#1675,#1673,#1099,.T.);
#1991=EDGE_CURVE('',#1674,#1676,#1100,.T.);
#1992=EDGE_CURVE('',#1676,#1677,#1101,.T.);
#1993=EDGE_CURVE('',#1677,#1675,#1102,.T.);
#1994=EDGE_CURVE('',#1676,#1678,#1103,.T.);
#1995=EDGE_CURVE('',#1678,#1679,#1104,.T.);
#1996=EDGE_CURVE('',#1679,#1677,#1105,.T.);
#1997=EDGE_CURVE('',#1678,#1668,#1106,.T.);
#1998=EDGE_CURVE('',#1671,#1679,#1107,.T.);
#1999=EDGE_CURVE('',#1680,#1680,#1445,.T.);
#2000=EDGE_CURVE('',#1681,#1681,#1446,.T.);
#2001=EDGE_CURVE('',#1682,#1682,#1447,.T.);
#2002=EDGE_CURVE('',#1682,#1681,#1108,.T.);
#2003=EDGE_CURVE('',#1683,#1683,#1448,.T.);
#2004=EDGE_CURVE('',#1683,#1682,#1109,.T.);
#2005=EDGE_CURVE('',#1684,#1684,#1449,.T.);
#2006=EDGE_CURVE('',#1684,#1683,#1110,.T.);
#2007=EDGE_CURVE('',#1685,#1685,#1450,.T.);
#2008=EDGE_CURVE('',#1686,#1686,#1451,.F.);
#2009=EDGE_CURVE('',#1686,#1685,#1111,.T.);
#2010=EDGE_CURVE('',#1680,#1686,#1112,.T.);
#2011=EDGE_CURVE('',#1687,#1687,#1452,.T.);
#2012=EDGE_CURVE('',#1687,#1688,#1113,.T.);
#2013=EDGE_CURVE('',#1688,#1688,#1453,.T.);
#2014=EDGE_CURVE('',#1689,#1689,#1454,.T.);
#2015=EDGE_CURVE('',#1689,#1690,#1114,.T.);
#2016=EDGE_CURVE('',#1690,#1690,#1455,.T.);
#2017=EDGE_CURVE('',#1691,#1691,#1456,.T.);
#2018=EDGE_CURVE('',#1691,#1692,#1115,.T.);
#2019=EDGE_CURVE('',#1692,#1692,#1457,.T.);
#2020=EDGE_CURVE('',#1693,#1693,#1458,.T.);
#2021=EDGE_CURVE('',#1693,#1694,#1116,.T.);
#2022=EDGE_CURVE('',#1694,#1694,#1459,.T.);
#2023=EDGE_CURVE('',#1695,#1695,#1460,.T.);
#2024=EDGE_CURVE('',#1695,#1696,#1117,.T.);
#2025=EDGE_CURVE('',#1696,#1696,#1461,.T.);
#2026=EDGE_CURVE('',#1697,#1697,#1462,.T.);
#2027=EDGE_CURVE('',#1698,#1698,#1463,.T.);
#2028=EDGE_CURVE('',#1698,#1697,#1118,.T.);
#2029=EDGE_CURVE('',#1699,#1699,#1464,.T.);
#2030=EDGE_CURVE('',#1699,#1700,#1119,.T.);
#2031=EDGE_CURVE('',#1700,#1700,#1465,.T.);
#2032=EDGE_CURVE('',#1701,#1702,#1120,.T.);
#2033=EDGE_CURVE('',#1703,#1701,#1466,.T.);
#2034=EDGE_CURVE('',#1704,#1703,#1121,.T.);
#2035=EDGE_CURVE('',#1702,#1704,#1467,.T.);
#2036=EDGE_CURVE('',#1705,#1703,#1122,.T.);
#2037=EDGE_CURVE('',#1706,#1705,#1123,.T.);
#2038=EDGE_CURVE('',#1704,#1706,#1124,.T.);
#2039=EDGE_CURVE('',#1701,#1707,#1125,.T.);
#2040=EDGE_CURVE('',#1707,#1705,#1468,.T.);
#2041=EDGE_CURVE('',#1708,#1702,#1126,.T.);
#2042=EDGE_CURVE('',#1707,#1708,#1127,.T.);
#2043=EDGE_CURVE('',#1708,#1706,#1469,.T.);
#2044=EDGE_CURVE('',#1709,#1709,#1470,.T.);
#2045=EDGE_CURVE('',#1710,#1710,#1471,.T.);
#2046=EDGE_CURVE('',#1711,#1711,#1472,.T.);
#2047=EDGE_CURVE('',#1709,#1710,#1128,.T.);
#2048=EDGE_CURVE('',#1711,#1712,#1129,.T.);
#2049=EDGE_CURVE('',#1712,#1712,#1473,.T.);
#2050=EDGE_CURVE('',#1713,#1714,#1474,.T.);
#2051=EDGE_CURVE('',#1714,#1713,#1475,.T.);
#2052=EDGE_CURVE('',#1714,#1715,#1476,.T.);
#2053=EDGE_CURVE('',#1716,#1715,#1477,.T.);
#2054=EDGE_CURVE('',#1715,#1716,#1478,.T.);
#2055=EDGE_CURVE('',#1716,#1717,#1130,.T.);
#2056=EDGE_CURVE('',#1717,#1717,#1479,.T.);
#2057=EDGE_CURVE('',#1718,#1718,#1480,.T.);
#2058=EDGE_CURVE('',#1718,#1719,#1131,.T.);
#2059=EDGE_CURVE('',#1719,#1719,#1481,.T.);
#2060=EDGE_CURVE('',#1719,#1720,#1132,.T.);
#2061=EDGE_CURVE('',#1720,#1720,#1482,.T.);
#2062=EDGE_CURVE('',#1721,#1721,#1483,.T.);
#2063=EDGE_CURVE('',#1721,#1713,#1133,.T.);
#2064=EDGE_CURVE('',#1722,#1722,#1484,.T.);
#2065=EDGE_CURVE('',#1722,#1718,#1134,.T.);
#2066=EDGE_CURVE('',#1723,#1724,#1485,.T.);
#2067=EDGE_CURVE('',#1724,#1723,#1486,.T.);
#2068=EDGE_CURVE('',#1724,#1725,#1487,.T.);
#2069=EDGE_CURVE('',#1726,#1725,#1488,.T.);
#2070=EDGE_CURVE('',#1725,#1726,#1489,.T.);
#2071=EDGE_CURVE('',#1727,#1727,#1490,.T.);
#2072=EDGE_CURVE('',#1727,#1726,#1135,.T.);
#2073=EDGE_CURVE('',#1728,#1728,#1491,.T.);
#2074=EDGE_CURVE('',#1729,#1729,#1492,.T.);
#2075=EDGE_CURVE('',#1730,#1730,#1493,.T.);
#2076=EDGE_CURVE('',#1730,#1728,#1136,.T.);
#2077=EDGE_CURVE('',#1731,#1731,#1494,.T.);
#2078=EDGE_CURVE('',#1731,#1730,#1137,.T.);
#2079=EDGE_CURVE('',#1732,#1732,#1495,.T.);
#2080=EDGE_CURVE('',#1732,#1731,#1138,.T.);
#2081=EDGE_CURVE('',#1723,#1729,#1139,.T.);
#2082=EDGE_CURVE('',#1733,#1734,#1496,.T.);
#2083=EDGE_CURVE('',#1735,#1736,#1497,.T.);
#2084=EDGE_CURVE('',#1737,#1738,#1498,.T.);
#2085=EDGE_CURVE('',#1739,#1740,#1499,.T.);
#2086=EDGE_CURVE('',#1741,#1742,#1500,.T.);
#2087=EDGE_CURVE('',#1743,#1744,#1501,.T.);
#2088=EDGE_CURVE('',#1745,#1746,#1502,.T.);
#2089=EDGE_CURVE('',#1747,#1748,#1503,.T.);
#2090=EDGE_CURVE('',#1749,#1750,#284,.T.);
#2091=EDGE_CURVE('',#1751,#1749,#1504,.T.);
#2092=EDGE_CURVE('',#1752,#1751,#285,.T.);
#2093=EDGE_CURVE('',#1750,#1752,#1505,.T.);
#2094=EDGE_CURVE('',#1753,#1751,#1506,.T.);
#2095=EDGE_CURVE('',#1753,#1754,#286,.T.);
#2096=EDGE_CURVE('',#1755,#1754,#1507,.T.);
#2097=EDGE_CURVE('',#1755,#1756,#287,.T.);
#2098=EDGE_CURVE('',#1757,#1756,#1508,.T.);
#2099=EDGE_CURVE('',#1757,#1758,#288,.T.);
#2100=EDGE_CURVE('',#1758,#1759,#1140,.T.);
#2101=EDGE_CURVE('',#1759,#1759,#1509,.T.);
#2102=EDGE_CURVE('',#1758,#1760,#289,.T.);
#2103=EDGE_CURVE('',#1761,#1760,#1510,.T.);
#2104=EDGE_CURVE('',#1761,#1762,#290,.T.);
#2105=EDGE_CURVE('',#1763,#1762,#1511,.T.);
#2106=EDGE_CURVE('',#1763,#1764,#291,.T.);
#2107=EDGE_CURVE('',#1765,#1764,#1512,.T.);
#2108=EDGE_CURVE('',#1765,#1766,#292,.T.);
#2109=EDGE_CURVE('',#1767,#1766,#1513,.T.);
#2110=EDGE_CURVE('',#1767,#1768,#293,.T.);
#2111=EDGE_CURVE('',#1752,#1768,#1514,.T.);
#2112=EDGE_CURVE('',#1749,#1769,#1515,.T.);
#2113=EDGE_CURVE('',#1769,#1753,#1516,.T.);
#2114=EDGE_CURVE('',#1770,#1769,#294,.T.);
#2115=EDGE_CURVE('',#1754,#1770,#1517,.T.);
#2116=EDGE_CURVE('',#1770,#1771,#1518,.T.);
#2117=EDGE_CURVE('',#1771,#1755,#1519,.T.);
#2118=EDGE_CURVE('',#1772,#1771,#295,.T.);
#2119=EDGE_CURVE('',#1756,#1772,#1520,.T.);
#2120=EDGE_CURVE('',#1772,#1773,#1521,.T.);
#2121=EDGE_CURVE('',#1773,#1757,#1522,.T.);
#2122=EDGE_CURVE('',#1774,#1775,#296,.T.);
#2123=EDGE_CURVE('',#1760,#1774,#1523,.T.);
#2124=EDGE_CURVE('',#1775,#1773,#297,.T.);
#2125=EDGE_CURVE('',#1774,#1776,#1524,.T.);
#2126=EDGE_CURVE('',#1776,#1761,#1525,.T.);
#2127=EDGE_CURVE('',#1777,#1776,#298,.T.);
#2128=EDGE_CURVE('',#1762,#1777,#1526,.T.);
#2129=EDGE_CURVE('',#1777,#1778,#1527,.T.);
#2130=EDGE_CURVE('',#1778,#1763,#1528,.T.);
#2131=EDGE_CURVE('',#1779,#1778,#299,.T.);
#2132=EDGE_CURVE('',#1764,#1779,#1529,.T.);
#2133=EDGE_CURVE('',#1779,#1780,#1530,.T.);
#2134=EDGE_CURVE('',#1780,#1765,#1531,.T.);
#2135=EDGE_CURVE('',#1781,#1780,#300,.T.);
#2136=EDGE_CURVE('',#1766,#1781,#1532,.T.);
#2137=EDGE_CURVE('',#1782,#1782,#1533,.T.);
#2138=EDGE_CURVE('',#1782,#1775,#1141,.T.);
#2139=EDGE_CURVE('',#1783,#1750,#1534,.T.);
#2140=EDGE_CURVE('',#1783,#1784,#301,.T.);
#2141=EDGE_CURVE('',#1781,#1784,#1535,.T.);
#2142=EDGE_CURVE('',#1768,#1783,#1536,.T.);
#2143=EDGE_CURVE('',#1784,#1767,#1537,.T.);
#2144=EDGE_CURVE('',#1785,#1785,#1538,.T.);
#2145=EDGE_CURVE('',#1786,#1786,#1539,.T.);
#2146=EDGE_CURVE('',#1787,#1787,#1540,.T.);
#2147=EDGE_CURVE('',#1787,#1785,#1142,.T.);
#2148=EDGE_CURVE('',#1788,#1788,#1541,.T.);
#2149=EDGE_CURVE('',#1788,#1786,#1143,.T.);
#2150=EDGE_CURVE('',#1789,#1789,#1542,.T.);
#2151=EDGE_CURVE('',#1790,#1790,#1543,.T.);
#2152=EDGE_CURVE('',#1791,#1791,#1544,.T.);
#2153=EDGE_CURVE('',#1791,#1789,#1144,.T.);
#2154=EDGE_CURVE('',#1792,#1792,#1545,.T.);
#2155=EDGE_CURVE('',#1792,#1790,#1145,.T.);
#2156=EDGE_CURVE('',#1793,#1793,#1546,.T.);
#2157=EDGE_CURVE('',#1793,#1794,#1146,.T.);
#2158=EDGE_CURVE('',#1794,#1794,#1547,.T.);
#2159=EDGE_CURVE('',#1795,#1795,#1548,.T.);
#2160=EDGE_CURVE('',#1796,#1796,#1549,.T.);
#2161=EDGE_CURVE('',#1796,#1797,#1147,.T.);
#2162=EDGE_CURVE('',#1797,#1797,#1550,.T.);
#2163=EDGE_CURVE('',#1798,#1798,#1551,.T.);
#2164=EDGE_CURVE('',#1799,#1799,#1552,.T.);
#2165=EDGE_CURVE('',#1799,#1800,#1148,.T.);
#2166=EDGE_CURVE('',#1800,#1800,#1553,.T.);
#2167=EDGE_CURVE('',#1801,#1801,#1554,.T.);
#2168=EDGE_CURVE('',#1802,#1802,#1555,.T.);
#2169=EDGE_CURVE('',#1802,#1803,#1149,.T.);
#2170=EDGE_CURVE('',#1803,#1803,#1556,.T.);
#2171=EDGE_CURVE('',#1804,#1804,#1557,.T.);
#2172=EDGE_CURVE('',#1805,#1805,#1558,.T.);
#2173=EDGE_CURVE('',#1805,#1795,#1150,.T.);
#2174=EDGE_CURVE('',#1806,#1806,#1559,.T.);
#2175=EDGE_CURVE('',#1806,#1798,#1151,.T.);
#2176=EDGE_CURVE('',#1807,#1807,#1560,.T.);
#2177=EDGE_CURVE('',#1807,#1801,#1152,.T.);
#2178=EDGE_CURVE('',#1808,#1808,#1561,.T.);
#2179=EDGE_CURVE('',#1808,#1804,#1153,.T.);
#2180=EDGE_CURVE('',#1809,#1809,#1562,.T.);
#2181=EDGE_CURVE('',#1809,#1810,#1154,.T.);
#2182=EDGE_CURVE('',#1810,#1810,#1563,.T.);
#2183=EDGE_CURVE('',#1811,#1811,#1564,.T.);
#2184=EDGE_CURVE('',#1812,#1812,#1565,.T.);
#2185=EDGE_CURVE('',#1812,#1811,#1155,.T.);
#2186=EDGE_CURVE('',#1813,#1813,#1566,.T.);
#2187=EDGE_CURVE('',#1813,#1814,#1156,.T.);
#2188=EDGE_CURVE('',#1814,#1814,#1567,.T.);
#2189=EDGE_CURVE('',#1815,#1816,#1157,.T.);
#2190=EDGE_CURVE('',#1816,#1817,#1158,.T.);
#2191=EDGE_CURVE('',#1817,#1818,#1159,.T.);
#2192=EDGE_CURVE('',#1815,#1818,#1160,.T.);
#2193=EDGE_CURVE('',#1816,#1819,#1161,.T.);
#2194=EDGE_CURVE('',#1819,#1820,#1162,.T.);
#2195=EDGE_CURVE('',#1820,#1817,#1163,.T.);
#2196=EDGE_CURVE('',#1819,#1821,#1164,.T.);
#2197=EDGE_CURVE('',#1821,#1822,#1165,.T.);
#2198=EDGE_CURVE('',#1822,#1820,#1166,.T.);
#2199=EDGE_CURVE('',#1821,#1823,#1167,.T.);
#2200=EDGE_CURVE('',#1823,#1824,#1168,.T.);
#2201=EDGE_CURVE('',#1824,#1822,#1169,.T.);
#2202=EDGE_CURVE('',#1823,#1825,#1170,.T.);
#2203=EDGE_CURVE('',#1825,#1826,#1171,.T.);
#2204=EDGE_CURVE('',#1826,#1824,#1172,.T.);
#2205=EDGE_CURVE('',#1825,#1815,#1173,.T.);
#2206=EDGE_CURVE('',#1818,#1826,#1174,.T.);
#2207=EDGE_CURVE('',#1827,#1827,#1568,.T.);
#2208=EDGE_CURVE('',#1828,#1828,#1569,.T.);
#2209=EDGE_CURVE('',#1829,#1829,#1570,.T.);
#2210=EDGE_CURVE('',#1829,#1828,#1175,.T.);
#2211=EDGE_CURVE('',#1830,#1830,#1571,.T.);
#2212=EDGE_CURVE('',#1830,#1829,#1176,.T.);
#2213=EDGE_CURVE('',#1831,#1831,#1572,.T.);
#2214=EDGE_CURVE('',#1831,#1830,#1177,.T.);
#2215=EDGE_CURVE('',#1832,#1832,#1573,.T.);
#2216=EDGE_CURVE('',#1833,#1833,#1574,.F.);
#2217=EDGE_CURVE('',#1833,#1832,#1178,.T.);
#2218=EDGE_CURVE('',#1827,#1833,#1179,.T.);
#2219=EDGE_CURVE('',#1834,#1835,#1180,.T.);
#2220=EDGE_CURVE('',#1836,#1834,#1575,.T.);
#2221=EDGE_CURVE('',#1837,#1836,#1181,.T.);
#2222=EDGE_CURVE('',#1837,#1835,#1576,.T.);
#2223=EDGE_CURVE('',#1838,#1835,#1182,.T.);
#2224=EDGE_CURVE('',#1839,#1838,#1183,.T.);
#2225=EDGE_CURVE('',#1834,#1839,#1184,.T.);
#2226=EDGE_CURVE('',#1837,#1840,#1185,.T.);
#2227=EDGE_CURVE('',#1838,#1840,#1577,.T.);
#2228=EDGE_CURVE('',#1841,#1841,#1578,.T.);
#2229=EDGE_CURVE('',#1842,#1842,#1579,.T.);
#2230=EDGE_CURVE('',#1843,#1843,#1580,.T.);
#2231=EDGE_CURVE('',#1844,#1844,#1581,.T.);
#2232=EDGE_CURVE('',#1841,#1843,#1186,.T.);
#2233=EDGE_CURVE('',#1844,#1845,#1187,.T.);
#2234=EDGE_CURVE('',#1845,#1845,#1582,.T.);
#2235=EDGE_CURVE('',#1846,#1836,#1188,.T.);
#2236=EDGE_CURVE('',#1840,#1846,#1189,.T.);
#2237=EDGE_CURVE('',#1839,#1846,#1583,.T.);
#2238=EDGE_CURVE('',#1847,#1847,#1584,.T.);
#2239=EDGE_CURVE('',#1848,#1848,#1585,.T.);
#2240=EDGE_CURVE('',#1842,#1847,#1190,.T.);
#2241=EDGE_CURVE('',#1848,#1849,#1191,.T.);
#2242=EDGE_CURVE('',#1849,#1849,#1586,.T.);
#2243=EDGE_CURVE('',#1850,#1850,#1587,.T.);
#2244=EDGE_CURVE('',#1850,#1851,#1192,.T.);
#2245=EDGE_CURVE('',#1851,#1851,#1588,.T.);
#2246=EDGE_CURVE('',#1852,#1852,#1589,.T.);
#2247=EDGE_CURVE('',#1852,#1853,#1193,.T.);
#2248=EDGE_CURVE('',#1853,#1853,#1590,.T.);
#2249=EDGE_CURVE('',#1854,#1855,#1194,.T.);
#2250=EDGE_CURVE('',#1854,#1855,#1591,.T.);
#2251=EDGE_CURVE('',#1856,#1854,#302,.T.);
#2252=EDGE_CURVE('',#1857,#1856,#1592,.T.);
#2253=EDGE_CURVE('',#1858,#1857,#303,.T.);
#2254=EDGE_CURVE('',#1858,#1859,#1195,.T.);
#2255=EDGE_CURVE('',#1860,#1859,#304,.T.);
#2256=EDGE_CURVE('',#1859,#1860,#305,.T.);
#2257=EDGE_CURVE('',#1855,#1858,#306,.T.);
#2258=EDGE_CURVE('',#1857,#1856,#1196,.T.);
#2259=EDGE_CURVE('',#1861,#1861,#1593,.T.);
#2260=EDGE_CURVE('',#1861,#1862,#1197,.T.);
#2261=EDGE_CURVE('',#1862,#1862,#1594,.T.);
#2262=EDGE_CURVE('',#1863,#1863,#1595,.T.);
#2263=EDGE_CURVE('',#1863,#1864,#1198,.T.);
#2264=EDGE_CURVE('',#1864,#1864,#1596,.T.);
#2265=EDGE_CURVE('',#1865,#1865,#1597,.T.);
#2266=EDGE_CURVE('',#1866,#1867,#1199,.T.);
#2267=EDGE_CURVE('',#1866,#1868,#1200,.T.);
#2268=EDGE_CURVE('',#1868,#1869,#1201,.T.);
#2269=EDGE_CURVE('',#1867,#1869,#1202,.T.);
#2270=EDGE_CURVE('',#1870,#1866,#1203,.T.);
#2271=EDGE_CURVE('',#1870,#1871,#1204,.T.);
#2272=EDGE_CURVE('',#1871,#1868,#1205,.T.);
#2273=EDGE_CURVE('',#1872,#1870,#1206,.T.);
#2274=EDGE_CURVE('',#1872,#1873,#1207,.T.);
#2275=EDGE_CURVE('',#1873,#1871,#1208,.T.);
#2276=EDGE_CURVE('',#1874,#1872,#1209,.T.);
#2277=EDGE_CURVE('',#1874,#1875,#1210,.T.);
#2278=EDGE_CURVE('',#1875,#1873,#1211,.T.);
#2279=EDGE_CURVE('',#1876,#1874,#1212,.T.);
#2280=EDGE_CURVE('',#1876,#1877,#1213,.T.);
#2281=EDGE_CURVE('',#1877,#1875,#1214,.T.);
#2282=EDGE_CURVE('',#1867,#1876,#1215,.T.);
#2283=EDGE_CURVE('',#1869,#1877,#1216,.T.);
#2284=EDGE_CURVE('',#1878,#1878,#1598,.T.);
#2285=EDGE_CURVE('',#1879,#1879,#1599,.T.);
#2286=EDGE_CURVE('',#1879,#1878,#1217,.T.);
#2287=EDGE_CURVE('',#1865,#1879,#1218,.T.);
#2288=ORIENTED_EDGE('',*,*,#1880,.F.);
#2289=ORIENTED_EDGE('',*,*,#1881,.T.);
#2290=ORIENTED_EDGE('',*,*,#1882,.F.);
#2291=ORIENTED_EDGE('',*,*,#1881,.F.);
#2292=ORIENTED_EDGE('',*,*,#1883,.F.);
#2293=ORIENTED_EDGE('',*,*,#1884,.T.);
#2294=ORIENTED_EDGE('',*,*,#1885,.F.);
#2295=ORIENTED_EDGE('',*,*,#1884,.F.);
#2296=ORIENTED_EDGE('',*,*,#1886,.F.);
#2297=ORIENTED_EDGE('',*,*,#1887,.T.);
#2298=ORIENTED_EDGE('',*,*,#1888,.F.);
#2299=ORIENTED_EDGE('',*,*,#1887,.F.);
#2300=ORIENTED_EDGE('',*,*,#1889,.F.);
#2301=ORIENTED_EDGE('',*,*,#1890,.T.);
#2302=ORIENTED_EDGE('',*,*,#1891,.F.);
#2303=ORIENTED_EDGE('',*,*,#1890,.F.);
#2304=ORIENTED_EDGE('',*,*,#1892,.F.);
#2305=ORIENTED_EDGE('',*,*,#1893,.T.);
#2306=ORIENTED_EDGE('',*,*,#1894,.F.);
#2307=ORIENTED_EDGE('',*,*,#1893,.F.);
#2308=ORIENTED_EDGE('',*,*,#1895,.F.);
#2309=ORIENTED_EDGE('',*,*,#1896,.T.);
#2310=ORIENTED_EDGE('',*,*,#1897,.F.);
#2311=ORIENTED_EDGE('',*,*,#1896,.F.);
#2312=ORIENTED_EDGE('',*,*,#1898,.F.);
#2313=ORIENTED_EDGE('',*,*,#1899,.T.);
#2314=ORIENTED_EDGE('',*,*,#1900,.F.);
#2315=ORIENTED_EDGE('',*,*,#1899,.F.);
#2316=ORIENTED_EDGE('',*,*,#1901,.F.);
#2317=ORIENTED_EDGE('',*,*,#1902,.T.);
#2318=ORIENTED_EDGE('',*,*,#1903,.F.);
#2319=ORIENTED_EDGE('',*,*,#1902,.F.);
#2320=ORIENTED_EDGE('',*,*,#1904,.T.);
#2321=ORIENTED_EDGE('',*,*,#1905,.T.);
#2322=ORIENTED_EDGE('',*,*,#1906,.F.);
#2323=ORIENTED_EDGE('',*,*,#1907,.F.);
#2324=ORIENTED_EDGE('',*,*,#1908,.T.);
#2325=ORIENTED_EDGE('',*,*,#1907,.T.);
#2326=ORIENTED_EDGE('',*,*,#1909,.F.);
#2327=ORIENTED_EDGE('',*,*,#1910,.F.);
#2328=ORIENTED_EDGE('',*,*,#1911,.T.);
#2329=ORIENTED_EDGE('',*,*,#1910,.T.);
#2330=ORIENTED_EDGE('',*,*,#1912,.F.);
#2331=ORIENTED_EDGE('',*,*,#1913,.F.);
#2332=ORIENTED_EDGE('',*,*,#1914,.T.);
#2333=ORIENTED_EDGE('',*,*,#1913,.T.);
#2334=ORIENTED_EDGE('',*,*,#1915,.F.);
#2335=ORIENTED_EDGE('',*,*,#1905,.F.);
#2336=ORIENTED_EDGE('',*,*,#1915,.T.);
#2337=ORIENTED_EDGE('',*,*,#1912,.T.);
#2338=ORIENTED_EDGE('',*,*,#1909,.T.);
#2339=ORIENTED_EDGE('',*,*,#1906,.T.);
#2340=ORIENTED_EDGE('',*,*,#1903,.T.);
#2341=ORIENTED_EDGE('',*,*,#1900,.T.);
#2342=ORIENTED_EDGE('',*,*,#1897,.T.);
#2343=ORIENTED_EDGE('',*,*,#1894,.T.);
#2344=ORIENTED_EDGE('',*,*,#1891,.T.);
#2345=ORIENTED_EDGE('',*,*,#1888,.T.);
#2346=ORIENTED_EDGE('',*,*,#1885,.T.);
#2347=ORIENTED_EDGE('',*,*,#1882,.T.);
#2348=ORIENTED_EDGE('',*,*,#1914,.F.);
#2349=ORIENTED_EDGE('',*,*,#1904,.F.);
#2350=ORIENTED_EDGE('',*,*,#1908,.F.);
#2351=ORIENTED_EDGE('',*,*,#1911,.F.);
#2352=ORIENTED_EDGE('',*,*,#1901,.T.);
#2353=ORIENTED_EDGE('',*,*,#1898,.T.);
#2354=ORIENTED_EDGE('',*,*,#1895,.T.);
#2355=ORIENTED_EDGE('',*,*,#1892,.T.);
#2356=ORIENTED_EDGE('',*,*,#1889,.T.);
#2357=ORIENTED_EDGE('',*,*,#1886,.T.);
#2358=ORIENTED_EDGE('',*,*,#1883,.T.);
#2359=ORIENTED_EDGE('',*,*,#1880,.T.);
#2360=ORIENTED_EDGE('',*,*,#1916,.F.);
#2361=ORIENTED_EDGE('',*,*,#1917,.F.);
#2362=ORIENTED_EDGE('',*,*,#1918,.T.);
#2363=ORIENTED_EDGE('',*,*,#1919,.F.);
#2364=ORIENTED_EDGE('',*,*,#1920,.F.);
#2365=ORIENTED_EDGE('',*,*,#1918,.F.);
#2366=ORIENTED_EDGE('',*,*,#1921,.F.);
#2367=ORIENTED_EDGE('',*,*,#1922,.T.);
#2368=ORIENTED_EDGE('',*,*,#1923,.F.);
#2369=ORIENTED_EDGE('',*,*,#1922,.F.);
#2370=ORIENTED_EDGE('',*,*,#1921,.T.);
#2371=ORIENTED_EDGE('',*,*,#1924,.F.);
#2372=ORIENTED_EDGE('',*,*,#1925,.T.);
#2373=ORIENTED_EDGE('',*,*,#1926,.F.);
#2374=ORIENTED_EDGE('',*,*,#1925,.F.);
#2375=ORIENTED_EDGE('',*,*,#1924,.T.);
#2376=ORIENTED_EDGE('',*,*,#1927,.F.);
#2377=ORIENTED_EDGE('',*,*,#1928,.T.);
#2378=ORIENTED_EDGE('',*,*,#1929,.F.);
#2379=ORIENTED_EDGE('',*,*,#1928,.F.);
#2380=ORIENTED_EDGE('',*,*,#1927,.T.);
#2381=ORIENTED_EDGE('',*,*,#1930,.F.);
#2382=ORIENTED_EDGE('',*,*,#1931,.T.);
#2383=ORIENTED_EDGE('',*,*,#1932,.F.);
#2384=ORIENTED_EDGE('',*,*,#1931,.F.);
#2385=ORIENTED_EDGE('',*,*,#1930,.T.);
#2386=ORIENTED_EDGE('',*,*,#1933,.F.);
#2387=ORIENTED_EDGE('',*,*,#1934,.F.);
#2388=ORIENTED_EDGE('',*,*,#1935,.F.);
#2389=ORIENTED_EDGE('',*,*,#1936,.F.);
#2390=ORIENTED_EDGE('',*,*,#1937,.F.);
#2391=ORIENTED_EDGE('',*,*,#1934,.T.);
#2392=ORIENTED_EDGE('',*,*,#1938,.F.);
#2393=ORIENTED_EDGE('',*,*,#1939,.T.);
#2394=ORIENTED_EDGE('',*,*,#1940,.F.);
#2395=ORIENTED_EDGE('',*,*,#1941,.F.);
#2396=ORIENTED_EDGE('',*,*,#1942,.F.);
#2397=ORIENTED_EDGE('',*,*,#1939,.F.);
#2398=ORIENTED_EDGE('',*,*,#1943,.F.);
#2399=ORIENTED_EDGE('',*,*,#1944,.T.);
#2400=ORIENTED_EDGE('',*,*,#1945,.F.);
#2401=ORIENTED_EDGE('',*,*,#1946,.F.);
#2402=ORIENTED_EDGE('',*,*,#1947,.F.);
#2403=ORIENTED_EDGE('',*,*,#1944,.F.);
#2404=ORIENTED_EDGE('',*,*,#1948,.F.);
#2405=ORIENTED_EDGE('',*,*,#1949,.T.);
#2406=ORIENTED_EDGE('',*,*,#1950,.F.);
#2407=ORIENTED_EDGE('',*,*,#1951,.F.);
#2408=ORIENTED_EDGE('',*,*,#1952,.F.);
#2409=ORIENTED_EDGE('',*,*,#1949,.F.);
#2410=ORIENTED_EDGE('',*,*,#1953,.F.);
#2411=ORIENTED_EDGE('',*,*,#1954,.T.);
#2412=ORIENTED_EDGE('',*,*,#1955,.T.);
#2413=ORIENTED_EDGE('',*,*,#1935,.T.);
#2414=ORIENTED_EDGE('',*,*,#1933,.T.);
#2415=ORIENTED_EDGE('',*,*,#1937,.T.);
#2416=ORIENTED_EDGE('',*,*,#1956,.T.);
#2417=ORIENTED_EDGE('',*,*,#1950,.T.);
#2418=ORIENTED_EDGE('',*,*,#1952,.T.);
#2419=ORIENTED_EDGE('',*,*,#1948,.T.);
#2420=ORIENTED_EDGE('',*,*,#1957,.T.);
#2421=ORIENTED_EDGE('',*,*,#1945,.T.);
#2422=ORIENTED_EDGE('',*,*,#1947,.T.);
#2423=ORIENTED_EDGE('',*,*,#1943,.T.);
#2424=ORIENTED_EDGE('',*,*,#1958,.T.);
#2425=ORIENTED_EDGE('',*,*,#1940,.T.);
#2426=ORIENTED_EDGE('',*,*,#1942,.T.);
#2427=ORIENTED_EDGE('',*,*,#1938,.T.);
#2428=ORIENTED_EDGE('',*,*,#1959,.T.);
#2429=ORIENTED_EDGE('',*,*,#1954,.F.);
#2430=ORIENTED_EDGE('',*,*,#1960,.T.);
#2431=ORIENTED_EDGE('',*,*,#1959,.F.);
#2432=ORIENTED_EDGE('',*,*,#1941,.T.);
#2433=ORIENTED_EDGE('',*,*,#1958,.F.);
#2434=ORIENTED_EDGE('',*,*,#1946,.T.);
#2435=ORIENTED_EDGE('',*,*,#1957,.F.);
#2436=ORIENTED_EDGE('',*,*,#1951,.T.);
#2437=ORIENTED_EDGE('',*,*,#1956,.F.);
#2438=ORIENTED_EDGE('',*,*,#1936,.T.);
#2439=ORIENTED_EDGE('',*,*,#1955,.F.);
#2440=ORIENTED_EDGE('',*,*,#1961,.T.);
#2441=ORIENTED_EDGE('',*,*,#1962,.T.);
#2442=ORIENTED_EDGE('',*,*,#1963,.T.);
#2443=ORIENTED_EDGE('',*,*,#1964,.T.);
#2444=ORIENTED_EDGE('',*,*,#1965,.F.);
#2445=ORIENTED_EDGE('',*,*,#1966,.T.);
#2446=ORIENTED_EDGE('',*,*,#1961,.F.);
#2447=ORIENTED_EDGE('',*,*,#1966,.F.);
#2448=ORIENTED_EDGE('',*,*,#1967,.F.);
#2449=ORIENTED_EDGE('',*,*,#1968,.T.);
#2450=ORIENTED_EDGE('',*,*,#1964,.F.);
#2451=ORIENTED_EDGE('',*,*,#1968,.F.);
#2452=ORIENTED_EDGE('',*,*,#1969,.F.);
#2453=ORIENTED_EDGE('',*,*,#1970,.T.);
#2454=ORIENTED_EDGE('',*,*,#1962,.F.);
#2455=ORIENTED_EDGE('',*,*,#1970,.F.);
#2456=ORIENTED_EDGE('',*,*,#1971,.F.);
#2457=ORIENTED_EDGE('',*,*,#1972,.T.);
#2458=ORIENTED_EDGE('',*,*,#1963,.F.);
#2459=ORIENTED_EDGE('',*,*,#1972,.F.);
#2460=ORIENTED_EDGE('',*,*,#1973,.F.);
#2461=ORIENTED_EDGE('',*,*,#1974,.T.);
#2462=ORIENTED_EDGE('',*,*,#1975,.F.);
#2463=ORIENTED_EDGE('',*,*,#1974,.F.);
#2464=ORIENTED_EDGE('',*,*,#1973,.T.);
#2465=ORIENTED_EDGE('',*,*,#1976,.F.);
#2466=ORIENTED_EDGE('',*,*,#1960,.F.);
#2467=ORIENTED_EDGE('',*,*,#1977,.T.);
#2468=ORIENTED_EDGE('',*,*,#1978,.T.);
#2469=ORIENTED_EDGE('',*,*,#1977,.F.);
#2470=ORIENTED_EDGE('',*,*,#1919,.T.);
#2471=ORIENTED_EDGE('',*,*,#1920,.T.);
#2472=ORIENTED_EDGE('',*,*,#1976,.T.);
#2473=ORIENTED_EDGE('',*,*,#1979,.T.);
#2474=ORIENTED_EDGE('',*,*,#1980,.T.);
#2475=ORIENTED_EDGE('',*,*,#1979,.F.);
#2476=ORIENTED_EDGE('',*,*,#1916,.T.);
#2477=ORIENTED_EDGE('',*,*,#1917,.T.);
#2478=ORIENTED_EDGE('',*,*,#1953,.T.);
#2479=ORIENTED_EDGE('',*,*,#1975,.T.);
#2480=ORIENTED_EDGE('',*,*,#1932,.T.);
#2481=ORIENTED_EDGE('',*,*,#1929,.T.);
#2482=ORIENTED_EDGE('',*,*,#1926,.T.);
#2483=ORIENTED_EDGE('',*,*,#1923,.T.);
#2484=ORIENTED_EDGE('',*,*,#1978,.F.);
#2485=ORIENTED_EDGE('',*,*,#1980,.F.);
#2486=ORIENTED_EDGE('',*,*,#1971,.T.);
#2487=ORIENTED_EDGE('',*,*,#1969,.T.);
#2488=ORIENTED_EDGE('',*,*,#1967,.T.);
#2489=ORIENTED_EDGE('',*,*,#1965,.T.);
#2490=ORIENTED_EDGE('',*,*,#1981,.T.);
#2491=ORIENTED_EDGE('',*,*,#1982,.T.);
#2492=ORIENTED_EDGE('',*,*,#1983,.T.);
#2493=ORIENTED_EDGE('',*,*,#1984,.F.);
#2494=ORIENTED_EDGE('',*,*,#1985,.T.);
#2495=ORIENTED_EDGE('',*,*,#1986,.T.);
#2496=ORIENTED_EDGE('',*,*,#1987,.T.);
#2497=ORIENTED_EDGE('',*,*,#1982,.F.);
#2498=ORIENTED_EDGE('',*,*,#1988,.T.);
#2499=ORIENTED_EDGE('',*,*,#1989,.T.);
#2500=ORIENTED_EDGE('',*,*,#1990,.T.);
#2501=ORIENTED_EDGE('',*,*,#1986,.F.);
#2502=ORIENTED_EDGE('',*,*,#1991,.T.);
#2503=ORIENTED_EDGE('',*,*,#1992,.T.);
#2504=ORIENTED_EDGE('',*,*,#1993,.T.);
#2505=ORIENTED_EDGE('',*,*,#1989,.F.);
#2506=ORIENTED_EDGE('',*,*,#1994,.T.);
#2507=ORIENTED_EDGE('',*,*,#1995,.T.);
#2508=ORIENTED_EDGE('',*,*,#1996,.T.);
#2509=ORIENTED_EDGE('',*,*,#1992,.F.);
#2510=ORIENTED_EDGE('',*,*,#1997,.T.);
#2511=ORIENTED_EDGE('',*,*,#1984,.T.);
#2512=ORIENTED_EDGE('',*,*,#1998,.T.);
#2513=ORIENTED_EDGE('',*,*,#1995,.F.);
#2514=ORIENTED_EDGE('',*,*,#1997,.F.);
#2515=ORIENTED_EDGE('',*,*,#1994,.F.);
#2516=ORIENTED_EDGE('',*,*,#1991,.F.);
#2517=ORIENTED_EDGE('',*,*,#1988,.F.);
#2518=ORIENTED_EDGE('',*,*,#1985,.F.);
#2519=ORIENTED_EDGE('',*,*,#1981,.F.);
#2520=ORIENTED_EDGE('',*,*,#1998,.F.);
#2521=ORIENTED_EDGE('',*,*,#1983,.F.);
#2522=ORIENTED_EDGE('',*,*,#1987,.F.);
#2523=ORIENTED_EDGE('',*,*,#1990,.F.);
#2524=ORIENTED_EDGE('',*,*,#1993,.F.);
#2525=ORIENTED_EDGE('',*,*,#1996,.F.);
#2526=ORIENTED_EDGE('',*,*,#1999,.F.);
#2527=ORIENTED_EDGE('',*,*,#2000,.F.);
#2528=ORIENTED_EDGE('',*,*,#2001,.F.);
#2529=ORIENTED_EDGE('',*,*,#2002,.T.);
#2530=ORIENTED_EDGE('',*,*,#2000,.T.);
#2531=ORIENTED_EDGE('',*,*,#2002,.F.);
#2532=ORIENTED_EDGE('',*,*,#2003,.F.);
#2533=ORIENTED_EDGE('',*,*,#2004,.T.);
#2534=ORIENTED_EDGE('',*,*,#2001,.T.);
#2535=ORIENTED_EDGE('',*,*,#2004,.F.);
#2536=ORIENTED_EDGE('',*,*,#2005,.F.);
#2537=ORIENTED_EDGE('',*,*,#2006,.T.);
#2538=ORIENTED_EDGE('',*,*,#2003,.T.);
#2539=ORIENTED_EDGE('',*,*,#2006,.F.);
#2540=ORIENTED_EDGE('',*,*,#2005,.T.);
#2541=ORIENTED_EDGE('',*,*,#2007,.F.);
#2542=ORIENTED_EDGE('',*,*,#2008,.F.);
#2543=ORIENTED_EDGE('',*,*,#2009,.T.);
#2544=ORIENTED_EDGE('',*,*,#2007,.T.);
#2545=ORIENTED_EDGE('',*,*,#2009,.F.);
#2546=ORIENTED_EDGE('',*,*,#1999,.T.);
#2547=ORIENTED_EDGE('',*,*,#2010,.T.);
#2548=ORIENTED_EDGE('',*,*,#2008,.T.);
#2549=ORIENTED_EDGE('',*,*,#2010,.F.);
#2550=ORIENTED_EDGE('',*,*,#2011,.F.);
#2551=ORIENTED_EDGE('',*,*,#2012,.T.);
#2552=ORIENTED_EDGE('',*,*,#2013,.F.);
#2553=ORIENTED_EDGE('',*,*,#2012,.F.);
#2554=ORIENTED_EDGE('',*,*,#2011,.T.);
#2555=ORIENTED_EDGE('',*,*,#2014,.F.);
#2556=ORIENTED_EDGE('',*,*,#2015,.T.);
#2557=ORIENTED_EDGE('',*,*,#2016,.F.);
#2558=ORIENTED_EDGE('',*,*,#2015,.F.);
#2559=ORIENTED_EDGE('',*,*,#2014,.T.);
#2560=ORIENTED_EDGE('',*,*,#2017,.F.);
#2561=ORIENTED_EDGE('',*,*,#2018,.T.);
#2562=ORIENTED_EDGE('',*,*,#2019,.F.);
#2563=ORIENTED_EDGE('',*,*,#2018,.F.);
#2564=ORIENTED_EDGE('',*,*,#2017,.T.);
#2565=ORIENTED_EDGE('',*,*,#2020,.F.);
#2566=ORIENTED_EDGE('',*,*,#2021,.T.);
#2567=ORIENTED_EDGE('',*,*,#2022,.F.);
#2568=ORIENTED_EDGE('',*,*,#2021,.F.);
#2569=ORIENTED_EDGE('',*,*,#2020,.T.);
#2570=ORIENTED_EDGE('',*,*,#2023,.F.);
#2571=ORIENTED_EDGE('',*,*,#2024,.T.);
#2572=ORIENTED_EDGE('',*,*,#2025,.F.);
#2573=ORIENTED_EDGE('',*,*,#2024,.F.);
#2574=ORIENTED_EDGE('',*,*,#2023,.T.);
#2575=ORIENTED_EDGE('',*,*,#2026,.F.);
#2576=ORIENTED_EDGE('',*,*,#2027,.F.);
#2577=ORIENTED_EDGE('',*,*,#2028,.T.);
#2578=ORIENTED_EDGE('',*,*,#2026,.T.);
#2579=ORIENTED_EDGE('',*,*,#2028,.F.);
#2580=ORIENTED_EDGE('',*,*,#2029,.F.);
#2581=ORIENTED_EDGE('',*,*,#2030,.T.);
#2582=ORIENTED_EDGE('',*,*,#2031,.T.);
#2583=ORIENTED_EDGE('',*,*,#2030,.F.);
#2584=ORIENTED_EDGE('',*,*,#2032,.F.);
#2585=ORIENTED_EDGE('',*,*,#2033,.F.);
#2586=ORIENTED_EDGE('',*,*,#2034,.F.);
#2587=ORIENTED_EDGE('',*,*,#2035,.F.);
#2588=ORIENTED_EDGE('',*,*,#2029,.T.);
#2589=ORIENTED_EDGE('',*,*,#2025,.T.);
#2590=ORIENTED_EDGE('',*,*,#2022,.T.);
#2591=ORIENTED_EDGE('',*,*,#2019,.T.);
#2592=ORIENTED_EDGE('',*,*,#2016,.T.);
#2593=ORIENTED_EDGE('',*,*,#2013,.T.);
#2594=ORIENTED_EDGE('',*,*,#2031,.F.);
#2595=ORIENTED_EDGE('',*,*,#2027,.T.);
#2596=ORIENTED_EDGE('',*,*,#2034,.T.);
#2597=ORIENTED_EDGE('',*,*,#2036,.F.);
#2598=ORIENTED_EDGE('',*,*,#2037,.F.);
#2599=ORIENTED_EDGE('',*,*,#2038,.F.);
#2600=ORIENTED_EDGE('',*,*,#2033,.T.);
#2601=ORIENTED_EDGE('',*,*,#2039,.T.);
#2602=ORIENTED_EDGE('',*,*,#2040,.T.);
#2603=ORIENTED_EDGE('',*,*,#2036,.T.);
#2604=ORIENTED_EDGE('',*,*,#2032,.T.);
#2605=ORIENTED_EDGE('',*,*,#2041,.F.);
#2606=ORIENTED_EDGE('',*,*,#2042,.F.);
#2607=ORIENTED_EDGE('',*,*,#2039,.F.);
#2608=ORIENTED_EDGE('',*,*,#2042,.T.);
#2609=ORIENTED_EDGE('',*,*,#2043,.T.);
#2610=ORIENTED_EDGE('',*,*,#2037,.T.);
#2611=ORIENTED_EDGE('',*,*,#2040,.F.);
#2612=ORIENTED_EDGE('',*,*,#2035,.T.);
#2613=ORIENTED_EDGE('',*,*,#2038,.T.);
#2614=ORIENTED_EDGE('',*,*,#2043,.F.);
#2615=ORIENTED_EDGE('',*,*,#2041,.T.);
#2616=ORIENTED_EDGE('',*,*,#2044,.T.);
#2617=ORIENTED_EDGE('',*,*,#2045,.F.);
#2618=ORIENTED_EDGE('',*,*,#2046,.F.);
#2619=ORIENTED_EDGE('',*,*,#2044,.F.);
#2620=ORIENTED_EDGE('',*,*,#2047,.T.);
#2621=ORIENTED_EDGE('',*,*,#2045,.T.);
#2622=ORIENTED_EDGE('',*,*,#2047,.F.);
#2623=ORIENTED_EDGE('',*,*,#2046,.T.);
#2624=ORIENTED_EDGE('',*,*,#2048,.T.);
#2625=ORIENTED_EDGE('',*,*,#2049,.T.);
#2626=ORIENTED_EDGE('',*,*,#2048,.F.);
#2627=ORIENTED_EDGE('',*,*,#2049,.F.);
#2628=ORIENTED_EDGE('',*,*,#2050,.F.);
#2629=ORIENTED_EDGE('',*,*,#2051,.F.);
#2630=ORIENTED_EDGE('',*,*,#2052,.T.);
#2631=ORIENTED_EDGE('',*,*,#2053,.F.);
#2632=ORIENTED_EDGE('',*,*,#2054,.F.);
#2633=ORIENTED_EDGE('',*,*,#2052,.F.);
#2634=ORIENTED_EDGE('',*,*,#2053,.T.);
#2635=ORIENTED_EDGE('',*,*,#2054,.T.);
#2636=ORIENTED_EDGE('',*,*,#2055,.T.);
#2637=ORIENTED_EDGE('',*,*,#2056,.T.);
#2638=ORIENTED_EDGE('',*,*,#2055,.F.);
#2639=ORIENTED_EDGE('',*,*,#2057,.T.);
#2640=ORIENTED_EDGE('',*,*,#2058,.T.);
#2641=ORIENTED_EDGE('',*,*,#2059,.F.);
#2642=ORIENTED_EDGE('',*,*,#2058,.F.);
#2643=ORIENTED_EDGE('',*,*,#2059,.T.);
#2644=ORIENTED_EDGE('',*,*,#2060,.T.);
#2645=ORIENTED_EDGE('',*,*,#2061,.F.);
#2646=ORIENTED_EDGE('',*,*,#2060,.F.);
#2647=ORIENTED_EDGE('',*,*,#2056,.F.);
#2648=ORIENTED_EDGE('',*,*,#2061,.T.);
#2649=ORIENTED_EDGE('',*,*,#2062,.F.);
#2650=ORIENTED_EDGE('',*,*,#2063,.T.);
#2651=ORIENTED_EDGE('',*,*,#2050,.T.);
#2652=ORIENTED_EDGE('',*,*,#2051,.T.);
#2653=ORIENTED_EDGE('',*,*,#2063,.F.);
#2654=ORIENTED_EDGE('',*,*,#2062,.T.);
#2655=ORIENTED_EDGE('',*,*,#2064,.F.);
#2656=ORIENTED_EDGE('',*,*,#2064,.T.);
#2657=ORIENTED_EDGE('',*,*,#2065,.T.);
#2658=ORIENTED_EDGE('',*,*,#2057,.F.);
#2659=ORIENTED_EDGE('',*,*,#2065,.F.);
#2660=ORIENTED_EDGE('',*,*,#2066,.F.);
#2661=ORIENTED_EDGE('',*,*,#2067,.F.);
#2662=ORIENTED_EDGE('',*,*,#2068,.T.);
#2663=ORIENTED_EDGE('',*,*,#2069,.F.);
#2664=ORIENTED_EDGE('',*,*,#2070,.F.);
#2665=ORIENTED_EDGE('',*,*,#2068,.F.);
#2666=ORIENTED_EDGE('',*,*,#2071,.T.);
#2667=ORIENTED_EDGE('',*,*,#2072,.T.);
#2668=ORIENTED_EDGE('',*,*,#2069,.T.);
#2669=ORIENTED_EDGE('',*,*,#2070,.T.);
#2670=ORIENTED_EDGE('',*,*,#2072,.F.);
#2671=ORIENTED_EDGE('',*,*,#2073,.F.);
#2672=ORIENTED_EDGE('',*,*,#2074,.T.);
#2673=ORIENTED_EDGE('',*,*,#2075,.F.);
#2674=ORIENTED_EDGE('',*,*,#2076,.T.);
#2675=ORIENTED_EDGE('',*,*,#2073,.T.);
#2676=ORIENTED_EDGE('',*,*,#2076,.F.);
#2677=ORIENTED_EDGE('',*,*,#2077,.F.);
#2678=ORIENTED_EDGE('',*,*,#2078,.T.);
#2679=ORIENTED_EDGE('',*,*,#2075,.T.);
#2680=ORIENTED_EDGE('',*,*,#2078,.F.);
#2681=ORIENTED_EDGE('',*,*,#2079,.F.);
#2682=ORIENTED_EDGE('',*,*,#2080,.T.);
#2683=ORIENTED_EDGE('',*,*,#2077,.T.);
#2684=ORIENTED_EDGE('',*,*,#2080,.F.);
#2685=ORIENTED_EDGE('',*,*,#2079,.T.);
#2686=ORIENTED_EDGE('',*,*,#2071,.F.);
#2687=ORIENTED_EDGE('',*,*,#2066,.T.);
#2688=ORIENTED_EDGE('',*,*,#2067,.T.);
#2689=ORIENTED_EDGE('',*,*,#2081,.T.);
#2690=ORIENTED_EDGE('',*,*,#2074,.F.);
#2691=ORIENTED_EDGE('',*,*,#2081,.F.);
#2692=ORIENTED_EDGE('',*,*,#2082,.T.);
#2693=ORIENTED_EDGE('',*,*,#2082,.F.);
#2694=ORIENTED_EDGE('',*,*,#2083,.T.);
#2695=ORIENTED_EDGE('',*,*,#2083,.F.);
#2696=ORIENTED_EDGE('',*,*,#2084,.T.);
#2697=ORIENTED_EDGE('',*,*,#2084,.F.);
#2698=ORIENTED_EDGE('',*,*,#2085,.T.);
#2699=ORIENTED_EDGE('',*,*,#2085,.F.);
#2700=ORIENTED_EDGE('',*,*,#2086,.T.);
#2701=ORIENTED_EDGE('',*,*,#2086,.F.);
#2702=ORIENTED_EDGE('',*,*,#2087,.T.);
#2703=ORIENTED_EDGE('',*,*,#2087,.F.);
#2704=ORIENTED_EDGE('',*,*,#2088,.T.);
#2705=ORIENTED_EDGE('',*,*,#2088,.F.);
#2706=ORIENTED_EDGE('',*,*,#2089,.T.);
#2707=ORIENTED_EDGE('',*,*,#2089,.F.);
#2708=ORIENTED_EDGE('',*,*,#2090,.F.);
#2709=ORIENTED_EDGE('',*,*,#2091,.F.);
#2710=ORIENTED_EDGE('',*,*,#2092,.F.);
#2711=ORIENTED_EDGE('',*,*,#2093,.F.);
#2712=ORIENTED_EDGE('',*,*,#2092,.T.);
#2713=ORIENTED_EDGE('',*,*,#2094,.F.);
#2714=ORIENTED_EDGE('',*,*,#2095,.T.);
#2715=ORIENTED_EDGE('',*,*,#2096,.F.);
#2716=ORIENTED_EDGE('',*,*,#2097,.T.);
#2717=ORIENTED_EDGE('',*,*,#2098,.F.);
#2718=ORIENTED_EDGE('',*,*,#2099,.T.);
#2719=ORIENTED_EDGE('',*,*,#2100,.T.);
#2720=ORIENTED_EDGE('',*,*,#2101,.F.);
#2721=ORIENTED_EDGE('',*,*,#2100,.F.);
#2722=ORIENTED_EDGE('',*,*,#2102,.T.);
#2723=ORIENTED_EDGE('',*,*,#2103,.F.);
#2724=ORIENTED_EDGE('',*,*,#2104,.T.);
#2725=ORIENTED_EDGE('',*,*,#2105,.F.);
#2726=ORIENTED_EDGE('',*,*,#2106,.T.);
#2727=ORIENTED_EDGE('',*,*,#2107,.F.);
#2728=ORIENTED_EDGE('',*,*,#2108,.T.);
#2729=ORIENTED_EDGE('',*,*,#2109,.F.);
#2730=ORIENTED_EDGE('',*,*,#2110,.T.);
#2731=ORIENTED_EDGE('',*,*,#2111,.F.);
#2732=ORIENTED_EDGE('',*,*,#2091,.T.);
#2733=ORIENTED_EDGE('',*,*,#2112,.T.);
#2734=ORIENTED_EDGE('',*,*,#2113,.T.);
#2735=ORIENTED_EDGE('',*,*,#2094,.T.);
#2736=ORIENTED_EDGE('',*,*,#2114,.F.);
#2737=ORIENTED_EDGE('',*,*,#2115,.F.);
#2738=ORIENTED_EDGE('',*,*,#2095,.F.);
#2739=ORIENTED_EDGE('',*,*,#2113,.F.);
#2740=ORIENTED_EDGE('',*,*,#2115,.T.);
#2741=ORIENTED_EDGE('',*,*,#2116,.T.);
#2742=ORIENTED_EDGE('',*,*,#2117,.T.);
#2743=ORIENTED_EDGE('',*,*,#2096,.T.);
#2744=ORIENTED_EDGE('',*,*,#2118,.F.);
#2745=ORIENTED_EDGE('',*,*,#2119,.F.);
#2746=ORIENTED_EDGE('',*,*,#2097,.F.);
#2747=ORIENTED_EDGE('',*,*,#2117,.F.);
#2748=ORIENTED_EDGE('',*,*,#2119,.T.);
#2749=ORIENTED_EDGE('',*,*,#2120,.T.);
#2750=ORIENTED_EDGE('',*,*,#2121,.T.);
#2751=ORIENTED_EDGE('',*,*,#2098,.T.);
#2752=ORIENTED_EDGE('',*,*,#2122,.F.);
#2753=ORIENTED_EDGE('',*,*,#2123,.F.);
#2754=ORIENTED_EDGE('',*,*,#2102,.F.);
#2755=ORIENTED_EDGE('',*,*,#2099,.F.);
#2756=ORIENTED_EDGE('',*,*,#2121,.F.);
#2757=ORIENTED_EDGE('',*,*,#2124,.F.);
#2758=ORIENTED_EDGE('',*,*,#2123,.T.);
#2759=ORIENTED_EDGE('',*,*,#2125,.T.);
#2760=ORIENTED_EDGE('',*,*,#2126,.T.);
#2761=ORIENTED_EDGE('',*,*,#2103,.T.);
#2762=ORIENTED_EDGE('',*,*,#2127,.F.);
#2763=ORIENTED_EDGE('',*,*,#2128,.F.);
#2764=ORIENTED_EDGE('',*,*,#2104,.F.);
#2765=ORIENTED_EDGE('',*,*,#2126,.F.);
#2766=ORIENTED_EDGE('',*,*,#2128,.T.);
#2767=ORIENTED_EDGE('',*,*,#2129,.T.);
#2768=ORIENTED_EDGE('',*,*,#2130,.T.);
#2769=ORIENTED_EDGE('',*,*,#2105,.T.);
#2770=ORIENTED_EDGE('',*,*,#2131,.F.);
#2771=ORIENTED_EDGE('',*,*,#2132,.F.);
#2772=ORIENTED_EDGE('',*,*,#2106,.F.);
#2773=ORIENTED_EDGE('',*,*,#2130,.F.);
#2774=ORIENTED_EDGE('',*,*,#2132,.T.);
#2775=ORIENTED_EDGE('',*,*,#2133,.T.);
#2776=ORIENTED_EDGE('',*,*,#2134,.T.);
#2777=ORIENTED_EDGE('',*,*,#2107,.T.);
#2778=ORIENTED_EDGE('',*,*,#2108,.F.);
#2779=ORIENTED_EDGE('',*,*,#2134,.F.);
#2780=ORIENTED_EDGE('',*,*,#2135,.F.);
#2781=ORIENTED_EDGE('',*,*,#2136,.F.);
#2782=ORIENTED_EDGE('',*,*,#2137,.F.);
#2783=ORIENTED_EDGE('',*,*,#2138,.T.);
#2784=ORIENTED_EDGE('',*,*,#2124,.T.);
#2785=ORIENTED_EDGE('',*,*,#2120,.F.);
#2786=ORIENTED_EDGE('',*,*,#2118,.T.);
#2787=ORIENTED_EDGE('',*,*,#2116,.F.);
#2788=ORIENTED_EDGE('',*,*,#2114,.T.);
#2789=ORIENTED_EDGE('',*,*,#2112,.F.);
#2790=ORIENTED_EDGE('',*,*,#2090,.T.);
#2791=ORIENTED_EDGE('',*,*,#2139,.F.);
#2792=ORIENTED_EDGE('',*,*,#2140,.T.);
#2793=ORIENTED_EDGE('',*,*,#2141,.F.);
#2794=ORIENTED_EDGE('',*,*,#2135,.T.);
#2795=ORIENTED_EDGE('',*,*,#2133,.F.);
#2796=ORIENTED_EDGE('',*,*,#2131,.T.);
#2797=ORIENTED_EDGE('',*,*,#2129,.F.);
#2798=ORIENTED_EDGE('',*,*,#2127,.T.);
#2799=ORIENTED_EDGE('',*,*,#2125,.F.);
#2800=ORIENTED_EDGE('',*,*,#2122,.T.);
#2801=ORIENTED_EDGE('',*,*,#2138,.F.);
#2802=ORIENTED_EDGE('',*,*,#2093,.T.);
#2803=ORIENTED_EDGE('',*,*,#2111,.T.);
#2804=ORIENTED_EDGE('',*,*,#2142,.T.);
#2805=ORIENTED_EDGE('',*,*,#2139,.T.);
#2806=ORIENTED_EDGE('',*,*,#2110,.F.);
#2807=ORIENTED_EDGE('',*,*,#2143,.F.);
#2808=ORIENTED_EDGE('',*,*,#2140,.F.);
#2809=ORIENTED_EDGE('',*,*,#2142,.F.);
#2810=ORIENTED_EDGE('',*,*,#2101,.T.);
#2811=ORIENTED_EDGE('',*,*,#2137,.T.);
#2812=ORIENTED_EDGE('',*,*,#2136,.T.);
#2813=ORIENTED_EDGE('',*,*,#2141,.T.);
#2814=ORIENTED_EDGE('',*,*,#2143,.T.);
#2815=ORIENTED_EDGE('',*,*,#2109,.T.);
#2816=ORIENTED_EDGE('',*,*,#2144,.F.);
#2817=ORIENTED_EDGE('',*,*,#2145,.T.);
#2818=ORIENTED_EDGE('',*,*,#2146,.F.);
#2819=ORIENTED_EDGE('',*,*,#2147,.T.);
#2820=ORIENTED_EDGE('',*,*,#2144,.T.);
#2821=ORIENTED_EDGE('',*,*,#2147,.F.);
#2822=ORIENTED_EDGE('',*,*,#2146,.T.);
#2823=ORIENTED_EDGE('',*,*,#2148,.F.);
#2824=ORIENTED_EDGE('',*,*,#2148,.T.);
#2825=ORIENTED_EDGE('',*,*,#2149,.T.);
#2826=ORIENTED_EDGE('',*,*,#2145,.F.);
#2827=ORIENTED_EDGE('',*,*,#2149,.F.);
#2828=ORIENTED_EDGE('',*,*,#2150,.F.);
#2829=ORIENTED_EDGE('',*,*,#2151,.T.);
#2830=ORIENTED_EDGE('',*,*,#2152,.F.);
#2831=ORIENTED_EDGE('',*,*,#2153,.T.);
#2832=ORIENTED_EDGE('',*,*,#2150,.T.);
#2833=ORIENTED_EDGE('',*,*,#2153,.F.);
#2834=ORIENTED_EDGE('',*,*,#2152,.T.);
#2835=ORIENTED_EDGE('',*,*,#2154,.F.);
#2836=ORIENTED_EDGE('',*,*,#2154,.T.);
#2837=ORIENTED_EDGE('',*,*,#2155,.T.);
#2838=ORIENTED_EDGE('',*,*,#2151,.F.);
#2839=ORIENTED_EDGE('',*,*,#2155,.F.);
#2840=ORIENTED_EDGE('',*,*,#2156,.F.);
#2841=ORIENTED_EDGE('',*,*,#2157,.T.);
#2842=ORIENTED_EDGE('',*,*,#2158,.F.);
#2843=ORIENTED_EDGE('',*,*,#2157,.F.);
#2844=ORIENTED_EDGE('',*,*,#2156,.T.);
#2845=ORIENTED_EDGE('',*,*,#2159,.F.);
#2846=ORIENTED_EDGE('',*,*,#2160,.F.);
#2847=ORIENTED_EDGE('',*,*,#2161,.T.);
#2848=ORIENTED_EDGE('',*,*,#2162,.F.);
#2849=ORIENTED_EDGE('',*,*,#2161,.F.);
#2850=ORIENTED_EDGE('',*,*,#2160,.T.);
#2851=ORIENTED_EDGE('',*,*,#2163,.F.);
#2852=ORIENTED_EDGE('',*,*,#2164,.F.);
#2853=ORIENTED_EDGE('',*,*,#2165,.T.);
#2854=ORIENTED_EDGE('',*,*,#2166,.F.);
#2855=ORIENTED_EDGE('',*,*,#2165,.F.);
#2856=ORIENTED_EDGE('',*,*,#2164,.T.);
#2857=ORIENTED_EDGE('',*,*,#2167,.F.);
#2858=ORIENTED_EDGE('',*,*,#2168,.F.);
#2859=ORIENTED_EDGE('',*,*,#2169,.T.);
#2860=ORIENTED_EDGE('',*,*,#2170,.F.);
#2861=ORIENTED_EDGE('',*,*,#2169,.F.);
#2862=ORIENTED_EDGE('',*,*,#2168,.T.);
#2863=ORIENTED_EDGE('',*,*,#2171,.F.);
#2864=ORIENTED_EDGE('',*,*,#2172,.F.);
#2865=ORIENTED_EDGE('',*,*,#2173,.T.);
#2866=ORIENTED_EDGE('',*,*,#2159,.T.);
#2867=ORIENTED_EDGE('',*,*,#2173,.F.);
#2868=ORIENTED_EDGE('',*,*,#2174,.F.);
#2869=ORIENTED_EDGE('',*,*,#2175,.T.);
#2870=ORIENTED_EDGE('',*,*,#2163,.T.);
#2871=ORIENTED_EDGE('',*,*,#2175,.F.);
#2872=ORIENTED_EDGE('',*,*,#2176,.F.);
#2873=ORIENTED_EDGE('',*,*,#2177,.T.);
#2874=ORIENTED_EDGE('',*,*,#2167,.T.);
#2875=ORIENTED_EDGE('',*,*,#2177,.F.);
#2876=ORIENTED_EDGE('',*,*,#2178,.F.);
#2877=ORIENTED_EDGE('',*,*,#2179,.T.);
#2878=ORIENTED_EDGE('',*,*,#2171,.T.);
#2879=ORIENTED_EDGE('',*,*,#2179,.F.);
#2880=ORIENTED_EDGE('',*,*,#2180,.F.);
#2881=ORIENTED_EDGE('',*,*,#2181,.T.);
#2882=ORIENTED_EDGE('',*,*,#2182,.T.);
#2883=ORIENTED_EDGE('',*,*,#2181,.F.);
#2884=ORIENTED_EDGE('',*,*,#2182,.F.);
#2885=ORIENTED_EDGE('',*,*,#2183,.F.);
#2886=ORIENTED_EDGE('',*,*,#2184,.F.);
#2887=ORIENTED_EDGE('',*,*,#2185,.T.);
#2888=ORIENTED_EDGE('',*,*,#2183,.T.);
#2889=ORIENTED_EDGE('',*,*,#2185,.F.);
#2890=ORIENTED_EDGE('',*,*,#2186,.F.);
#2891=ORIENTED_EDGE('',*,*,#2187,.T.);
#2892=ORIENTED_EDGE('',*,*,#2188,.T.);
#2893=ORIENTED_EDGE('',*,*,#2187,.F.);
#2894=ORIENTED_EDGE('',*,*,#2186,.T.);
#2895=ORIENTED_EDGE('',*,*,#2184,.T.);
#2896=ORIENTED_EDGE('',*,*,#2170,.T.);
#2897=ORIENTED_EDGE('',*,*,#2166,.T.);
#2898=ORIENTED_EDGE('',*,*,#2162,.T.);
#2899=ORIENTED_EDGE('',*,*,#2158,.T.);
#2900=ORIENTED_EDGE('',*,*,#2188,.F.);
#2901=ORIENTED_EDGE('',*,*,#2180,.T.);
#2902=ORIENTED_EDGE('',*,*,#2178,.T.);
#2903=ORIENTED_EDGE('',*,*,#2176,.T.);
#2904=ORIENTED_EDGE('',*,*,#2174,.T.);
#2905=ORIENTED_EDGE('',*,*,#2172,.T.);
#2906=ORIENTED_EDGE('',*,*,#2189,.T.);
#2907=ORIENTED_EDGE('',*,*,#2190,.T.);
#2908=ORIENTED_EDGE('',*,*,#2191,.T.);
#2909=ORIENTED_EDGE('',*,*,#2192,.F.);
#2910=ORIENTED_EDGE('',*,*,#2193,.T.);
#2911=ORIENTED_EDGE('',*,*,#2194,.T.);
#2912=ORIENTED_EDGE('',*,*,#2195,.T.);
#2913=ORIENTED_EDGE('',*,*,#2190,.F.);
#2914=ORIENTED_EDGE('',*,*,#2196,.T.);
#2915=ORIENTED_EDGE('',*,*,#2197,.T.);
#2916=ORIENTED_EDGE('',*,*,#2198,.T.);
#2917=ORIENTED_EDGE('',*,*,#2194,.F.);
#2918=ORIENTED_EDGE('',*,*,#2199,.T.);
#2919=ORIENTED_EDGE('',*,*,#2200,.T.);
#2920=ORIENTED_EDGE('',*,*,#2201,.T.);
#2921=ORIENTED_EDGE('',*,*,#2197,.F.);
#2922=ORIENTED_EDGE('',*,*,#2202,.T.);
#2923=ORIENTED_EDGE('',*,*,#2203,.T.);
#2924=ORIENTED_EDGE('',*,*,#2204,.T.);
#2925=ORIENTED_EDGE('',*,*,#2200,.F.);
#2926=ORIENTED_EDGE('',*,*,#2205,.T.);
#2927=ORIENTED_EDGE('',*,*,#2192,.T.);
#2928=ORIENTED_EDGE('',*,*,#2206,.T.);
#2929=ORIENTED_EDGE('',*,*,#2203,.F.);
#2930=ORIENTED_EDGE('',*,*,#2205,.F.);
#2931=ORIENTED_EDGE('',*,*,#2202,.F.);
#2932=ORIENTED_EDGE('',*,*,#2199,.F.);
#2933=ORIENTED_EDGE('',*,*,#2196,.F.);
#2934=ORIENTED_EDGE('',*,*,#2193,.F.);
#2935=ORIENTED_EDGE('',*,*,#2189,.F.);
#2936=ORIENTED_EDGE('',*,*,#2206,.F.);
#2937=ORIENTED_EDGE('',*,*,#2191,.F.);
#2938=ORIENTED_EDGE('',*,*,#2195,.F.);
#2939=ORIENTED_EDGE('',*,*,#2198,.F.);
#2940=ORIENTED_EDGE('',*,*,#2201,.F.);
#2941=ORIENTED_EDGE('',*,*,#2204,.F.);
#2942=ORIENTED_EDGE('',*,*,#2207,.F.);
#2943=ORIENTED_EDGE('',*,*,#2208,.F.);
#2944=ORIENTED_EDGE('',*,*,#2209,.F.);
#2945=ORIENTED_EDGE('',*,*,#2210,.T.);
#2946=ORIENTED_EDGE('',*,*,#2208,.T.);
#2947=ORIENTED_EDGE('',*,*,#2210,.F.);
#2948=ORIENTED_EDGE('',*,*,#2211,.F.);
#2949=ORIENTED_EDGE('',*,*,#2212,.T.);
#2950=ORIENTED_EDGE('',*,*,#2209,.T.);
#2951=ORIENTED_EDGE('',*,*,#2212,.F.);
#2952=ORIENTED_EDGE('',*,*,#2213,.F.);
#2953=ORIENTED_EDGE('',*,*,#2214,.T.);
#2954=ORIENTED_EDGE('',*,*,#2211,.T.);
#2955=ORIENTED_EDGE('',*,*,#2214,.F.);
#2956=ORIENTED_EDGE('',*,*,#2213,.T.);
#2957=ORIENTED_EDGE('',*,*,#2215,.F.);
#2958=ORIENTED_EDGE('',*,*,#2216,.F.);
#2959=ORIENTED_EDGE('',*,*,#2217,.T.);
#2960=ORIENTED_EDGE('',*,*,#2215,.T.);
#2961=ORIENTED_EDGE('',*,*,#2217,.F.);
#2962=ORIENTED_EDGE('',*,*,#2207,.T.);
#2963=ORIENTED_EDGE('',*,*,#2218,.T.);
#2964=ORIENTED_EDGE('',*,*,#2216,.T.);
#2965=ORIENTED_EDGE('',*,*,#2218,.F.);
#2966=ORIENTED_EDGE('',*,*,#2219,.F.);
#2967=ORIENTED_EDGE('',*,*,#2220,.F.);
#2968=ORIENTED_EDGE('',*,*,#2221,.F.);
#2969=ORIENTED_EDGE('',*,*,#2222,.T.);
#2970=ORIENTED_EDGE('',*,*,#2219,.T.);
#2971=ORIENTED_EDGE('',*,*,#2223,.F.);
#2972=ORIENTED_EDGE('',*,*,#2224,.F.);
#2973=ORIENTED_EDGE('',*,*,#2225,.F.);
#2974=ORIENTED_EDGE('',*,*,#2222,.F.);
#2975=ORIENTED_EDGE('',*,*,#2226,.T.);
#2976=ORIENTED_EDGE('',*,*,#2227,.F.);
#2977=ORIENTED_EDGE('',*,*,#2223,.T.);
#2978=ORIENTED_EDGE('',*,*,#2228,.T.);
#2979=ORIENTED_EDGE('',*,*,#2229,.T.);
#2980=ORIENTED_EDGE('',*,*,#2230,.F.);
#2981=ORIENTED_EDGE('',*,*,#2231,.F.);
#2982=ORIENTED_EDGE('',*,*,#2228,.F.);
#2983=ORIENTED_EDGE('',*,*,#2232,.T.);
#2984=ORIENTED_EDGE('',*,*,#2230,.T.);
#2985=ORIENTED_EDGE('',*,*,#2232,.F.);
#2986=ORIENTED_EDGE('',*,*,#2231,.T.);
#2987=ORIENTED_EDGE('',*,*,#2233,.T.);
#2988=ORIENTED_EDGE('',*,*,#2234,.T.);
#2989=ORIENTED_EDGE('',*,*,#2233,.F.);
#2990=ORIENTED_EDGE('',*,*,#2234,.F.);
#2991=ORIENTED_EDGE('',*,*,#2221,.T.);
#2992=ORIENTED_EDGE('',*,*,#2235,.F.);
#2993=ORIENTED_EDGE('',*,*,#2236,.F.);
#2994=ORIENTED_EDGE('',*,*,#2226,.F.);
#2995=ORIENTED_EDGE('',*,*,#2224,.T.);
#2996=ORIENTED_EDGE('',*,*,#2227,.T.);
#2997=ORIENTED_EDGE('',*,*,#2236,.T.);
#2998=ORIENTED_EDGE('',*,*,#2237,.F.);
#2999=ORIENTED_EDGE('',*,*,#2238,.F.);
#3000=ORIENTED_EDGE('',*,*,#2239,.F.);
#3001=ORIENTED_EDGE('',*,*,#2229,.F.);
#3002=ORIENTED_EDGE('',*,*,#2240,.T.);
#3003=ORIENTED_EDGE('',*,*,#2238,.T.);
#3004=ORIENTED_EDGE('',*,*,#2240,.F.);
#3005=ORIENTED_EDGE('',*,*,#2239,.T.);
#3006=ORIENTED_EDGE('',*,*,#2241,.T.);
#3007=ORIENTED_EDGE('',*,*,#2242,.T.);
#3008=ORIENTED_EDGE('',*,*,#2241,.F.);
#3009=ORIENTED_EDGE('',*,*,#2225,.T.);
#3010=ORIENTED_EDGE('',*,*,#2237,.T.);
#3011=ORIENTED_EDGE('',*,*,#2235,.T.);
#3012=ORIENTED_EDGE('',*,*,#2220,.T.);
#3013=ORIENTED_EDGE('',*,*,#2242,.F.);
#3014=ORIENTED_EDGE('',*,*,#2243,.F.);
#3015=ORIENTED_EDGE('',*,*,#2244,.T.);
#3016=ORIENTED_EDGE('',*,*,#2245,.T.);
#3017=ORIENTED_EDGE('',*,*,#2244,.F.);
#3018=ORIENTED_EDGE('',*,*,#2246,.F.);
#3019=ORIENTED_EDGE('',*,*,#2247,.T.);
#3020=ORIENTED_EDGE('',*,*,#2248,.T.);
#3021=ORIENTED_EDGE('',*,*,#2247,.F.);
#3022=ORIENTED_EDGE('',*,*,#2246,.T.);
#3023=ORIENTED_EDGE('',*,*,#2243,.T.);
#3024=ORIENTED_EDGE('',*,*,#2248,.F.);
#3025=ORIENTED_EDGE('',*,*,#2245,.F.);
#3026=ORIENTED_EDGE('',*,*,#2249,.F.);
#3027=ORIENTED_EDGE('',*,*,#2250,.T.);
#3028=ORIENTED_EDGE('',*,*,#2251,.F.);
#3029=ORIENTED_EDGE('',*,*,#2252,.F.);
#3030=ORIENTED_EDGE('',*,*,#2253,.F.);
#3031=ORIENTED_EDGE('',*,*,#2254,.T.);
#3032=ORIENTED_EDGE('',*,*,#2255,.F.);
#3033=ORIENTED_EDGE('',*,*,#2256,.F.);
#3034=ORIENTED_EDGE('',*,*,#2254,.F.);
#3035=ORIENTED_EDGE('',*,*,#2257,.F.);
#3036=ORIENTED_EDGE('',*,*,#2250,.F.);
#3037=ORIENTED_EDGE('',*,*,#2258,.F.);
#3038=ORIENTED_EDGE('',*,*,#2252,.T.);
#3039=ORIENTED_EDGE('',*,*,#2259,.F.);
#3040=ORIENTED_EDGE('',*,*,#2260,.T.);
#3041=ORIENTED_EDGE('',*,*,#2261,.T.);
#3042=ORIENTED_EDGE('',*,*,#2260,.F.);
#3043=ORIENTED_EDGE('',*,*,#2257,.T.);
#3044=ORIENTED_EDGE('',*,*,#2253,.T.);
#3045=ORIENTED_EDGE('',*,*,#2258,.T.);
#3046=ORIENTED_EDGE('',*,*,#2251,.T.);
#3047=ORIENTED_EDGE('',*,*,#2249,.T.);
#3048=ORIENTED_EDGE('',*,*,#2262,.F.);
#3049=ORIENTED_EDGE('',*,*,#2263,.T.);
#3050=ORIENTED_EDGE('',*,*,#2264,.T.);
#3051=ORIENTED_EDGE('',*,*,#2263,.F.);
#3052=ORIENTED_EDGE('',*,*,#2255,.T.);
#3053=ORIENTED_EDGE('',*,*,#2256,.T.);
#3054=ORIENTED_EDGE('',*,*,#2262,.T.);
#3055=ORIENTED_EDGE('',*,*,#2259,.T.);
#3056=ORIENTED_EDGE('',*,*,#2264,.F.);
#3057=ORIENTED_EDGE('',*,*,#2261,.F.);
#3058=ORIENTED_EDGE('',*,*,#2265,.F.);
#3059=ORIENTED_EDGE('',*,*,#2266,.F.);
#3060=ORIENTED_EDGE('',*,*,#2267,.T.);
#3061=ORIENTED_EDGE('',*,*,#2268,.T.);
#3062=ORIENTED_EDGE('',*,*,#2269,.F.);
#3063=ORIENTED_EDGE('',*,*,#2270,.F.);
#3064=ORIENTED_EDGE('',*,*,#2271,.T.);
#3065=ORIENTED_EDGE('',*,*,#2272,.T.);
#3066=ORIENTED_EDGE('',*,*,#2267,.F.);
#3067=ORIENTED_EDGE('',*,*,#2273,.F.);
#3068=ORIENTED_EDGE('',*,*,#2274,.T.);
#3069=ORIENTED_EDGE('',*,*,#2275,.T.);
#3070=ORIENTED_EDGE('',*,*,#2271,.F.);
#3071=ORIENTED_EDGE('',*,*,#2276,.F.);
#3072=ORIENTED_EDGE('',*,*,#2277,.T.);
#3073=ORIENTED_EDGE('',*,*,#2278,.T.);
#3074=ORIENTED_EDGE('',*,*,#2274,.F.);
#3075=ORIENTED_EDGE('',*,*,#2279,.F.);
#3076=ORIENTED_EDGE('',*,*,#2280,.T.);
#3077=ORIENTED_EDGE('',*,*,#2281,.T.);
#3078=ORIENTED_EDGE('',*,*,#2277,.F.);
#3079=ORIENTED_EDGE('',*,*,#2282,.F.);
#3080=ORIENTED_EDGE('',*,*,#2269,.T.);
#3081=ORIENTED_EDGE('',*,*,#2283,.T.);
#3082=ORIENTED_EDGE('',*,*,#2280,.F.);
#3083=ORIENTED_EDGE('',*,*,#2283,.F.);
#3084=ORIENTED_EDGE('',*,*,#2268,.F.);
#3085=ORIENTED_EDGE('',*,*,#2272,.F.);
#3086=ORIENTED_EDGE('',*,*,#2275,.F.);
#3087=ORIENTED_EDGE('',*,*,#2278,.F.);
#3088=ORIENTED_EDGE('',*,*,#2281,.F.);
#3089=ORIENTED_EDGE('',*,*,#2284,.F.);
#3090=ORIENTED_EDGE('',*,*,#2266,.T.);
#3091=ORIENTED_EDGE('',*,*,#2282,.T.);
#3092=ORIENTED_EDGE('',*,*,#2279,.T.);
#3093=ORIENTED_EDGE('',*,*,#2276,.T.);
#3094=ORIENTED_EDGE('',*,*,#2273,.T.);
#3095=ORIENTED_EDGE('',*,*,#2270,.T.);
#3096=ORIENTED_EDGE('',*,*,#2285,.F.);
#3097=ORIENTED_EDGE('',*,*,#2286,.T.);
#3098=ORIENTED_EDGE('',*,*,#2284,.T.);
#3099=ORIENTED_EDGE('',*,*,#2286,.F.);
#3100=ORIENTED_EDGE('',*,*,#2265,.T.);
#3101=ORIENTED_EDGE('',*,*,#2287,.T.);
#3102=ORIENTED_EDGE('',*,*,#2285,.T.);
#3103=ORIENTED_EDGE('',*,*,#2287,.F.);
#3104=CYLINDRICAL_SURFACE('',#3575,0.21);
#3105=CYLINDRICAL_SURFACE('',#3578,0.21);
#3106=CYLINDRICAL_SURFACE('',#3581,0.210000000000001);
#3107=CYLINDRICAL_SURFACE('',#3584,0.210000000000001);
#3108=CYLINDRICAL_SURFACE('',#3587,0.21);
#3109=CYLINDRICAL_SURFACE('',#3590,0.21);
#3110=CYLINDRICAL_SURFACE('',#3593,0.21);
#3111=CYLINDRICAL_SURFACE('',#3596,0.21);
#3112=CYLINDRICAL_SURFACE('',#3606,0.25);
#3113=CYLINDRICAL_SURFACE('',#3607,0.165);
#3114=CYLINDRICAL_SURFACE('',#3611,0.165);
#3115=CYLINDRICAL_SURFACE('',#3615,0.165);
#3116=CYLINDRICAL_SURFACE('',#3619,0.165);
#3117=CYLINDRICAL_SURFACE('',#3626,0.525);
#3118=CYLINDRICAL_SURFACE('',#3628,0.525);
#3119=CYLINDRICAL_SURFACE('',#3633,0.525);
#3120=CYLINDRICAL_SURFACE('',#3638,0.525);
#3121=CYLINDRICAL_SURFACE('',#3643,2.2);
#3122=CYLINDRICAL_SURFACE('',#3656,0.275);
#3123=CYLINDRICAL_SURFACE('',#3658,0.275);
#3124=CYLINDRICAL_SURFACE('',#3660,0.275);
#3125=CYLINDRICAL_SURFACE('',#3662,0.275);
#3126=CYLINDRICAL_SURFACE('',#3664,1.5);
#3127=CYLINDRICAL_SURFACE('',#3669,3.);
#3128=CYLINDRICAL_SURFACE('',#3671,1.02);
#3129=CYLINDRICAL_SURFACE('',#3690,0.425);
#3130=CYLINDRICAL_SURFACE('',#3698,0.24505);
#3131=CYLINDRICAL_SURFACE('',#3702,0.165);
#3132=CYLINDRICAL_SURFACE('',#3706,0.165);
#3133=CYLINDRICAL_SURFACE('',#3710,0.165);
#3134=CYLINDRICAL_SURFACE('',#3714,0.165);
#3135=CYLINDRICAL_SURFACE('',#3718,1.5);
#3136=CYLINDRICAL_SURFACE('',#3723,1.02);
#3137=CYLINDRICAL_SURFACE('',#3725,2.2);
#3138=CYLINDRICAL_SURFACE('',#3736,1.);
#3139=CYLINDRICAL_SURFACE('',#3743,0.7);
#3140=CYLINDRICAL_SURFACE('',#3744,0.5);
#3141=CYLINDRICAL_SURFACE('',#3755,0.976185);
#3142=CYLINDRICAL_SURFACE('',#3757,0.5);
#3143=CYLINDRICAL_SURFACE('',#3763,0.976185);
#3144=CYLINDRICAL_SURFACE('',#3775,1.023815);
#3145=CYLINDRICAL_SURFACE('',#3782,1.5);
#3146=CYLINDRICAL_SURFACE('',#3787,1.023815);
#3147=CYLINDRICAL_SURFACE('',#3809,1.019052);
#3148=CYLINDRICAL_SURFACE('',#3849,0.980948);
#3149=CYLINDRICAL_SURFACE('',#3863,1.013815);
#3150=CYLINDRICAL_SURFACE('',#3867,0.991185);
#3151=CYLINDRICAL_SURFACE('',#3871,1.013815);
#3152=CYLINDRICAL_SURFACE('',#3875,0.991185);
#3153=CYLINDRICAL_SURFACE('',#3882,0.375);
#3154=CYLINDRICAL_SURFACE('',#3887,0.375);
#3155=CYLINDRICAL_SURFACE('',#3892,0.375);
#3156=CYLINDRICAL_SURFACE('',#3897,0.375);
#3157=CYLINDRICAL_SURFACE('',#3902,0.225);
#3158=CYLINDRICAL_SURFACE('',#3904,0.225);
#3159=CYLINDRICAL_SURFACE('',#3906,0.225);
#3160=CYLINDRICAL_SURFACE('',#3908,0.225);
#3161=CYLINDRICAL_SURFACE('',#3910,1.49);
#3162=CYLINDRICAL_SURFACE('',#3915,0.71);
#3163=CYLINDRICAL_SURFACE('',#3917,2.2);
#3164=CYLINDRICAL_SURFACE('',#3937,0.35);
#3165=CYLINDRICAL_SURFACE('',#3945,0.1954);
#3166=CYLINDRICAL_SURFACE('',#3971,1.);
#3167=CYLINDRICAL_SURFACE('',#3982,0.699999999999999);
#3168=CYLINDRICAL_SURFACE('',#3983,0.5);
#3169=CYLINDRICAL_SURFACE('',#3987,1.);
#3170=CYLINDRICAL_SURFACE('',#3992,0.7);
#3171=CYLINDRICAL_SURFACE('',#3993,0.5);
#3172=CYLINDRICAL_SURFACE('',#3998,0.505);
#3173=CYLINDRICAL_SURFACE('',#4001,0.7);
#3174=CYLINDRICAL_SURFACE('',#4009,0.165);
#3175=CYLINDRICAL_SURFACE('',#4012,0.505);
#3176=CYLINDRICAL_SURFACE('',#4015,0.9);
#3177=CYLINDRICAL_SURFACE('',#4034,0.1954);
#3178=ADVANCED_FACE('',(#562),#3104,.F.);
#3179=ADVANCED_FACE('',(#563),#3105,.F.);
#3180=ADVANCED_FACE('',(#564),#3106,.F.);
#3181=ADVANCED_FACE('',(#565),#3107,.F.);
#3182=ADVANCED_FACE('',(#566),#3108,.F.);
#3183=ADVANCED_FACE('',(#567),#3109,.F.);
#3184=ADVANCED_FACE('',(#568),#3110,.F.);
#3185=ADVANCED_FACE('',(#569),#3111,.F.);
#3186=ADVANCED_FACE('',(#570),#462,.T.);
#3187=ADVANCED_FACE('',(#571),#463,.T.);
#3188=ADVANCED_FACE('',(#572),#464,.T.);
#3189=ADVANCED_FACE('',(#573),#465,.T.);
#3190=ADVANCED_FACE('',(#574,#381,#382,#383,#384,#385,#386,#387,#388),#466,
 .T.);
#3191=ADVANCED_FACE('',(#575,#389,#390,#391,#392,#393,#394,#395,#396),#467,
 .F.);
#3192=ADVANCED_FACE('',(#576),#3112,.F.);
#3193=ADVANCED_FACE('',(#577),#3113,.F.);
#3194=ADVANCED_FACE('',(#578),#468,.T.);
#3195=ADVANCED_FACE('',(#579),#3114,.F.);
#3196=ADVANCED_FACE('',(#580),#469,.T.);
#3197=ADVANCED_FACE('',(#581),#3115,.F.);
#3198=ADVANCED_FACE('',(#582),#470,.T.);
#3199=ADVANCED_FACE('',(#583),#3116,.F.);
#3200=ADVANCED_FACE('',(#584),#471,.T.);
#3201=ADVANCED_FACE('',(#585),#472,.F.);
#3202=ADVANCED_FACE('',(#586),#3117,.F.);
#3203=ADVANCED_FACE('',(#587),#3118,.F.);
#3204=ADVANCED_FACE('',(#588),#473,.F.);
#3205=ADVANCED_FACE('',(#589),#3119,.F.);
#3206=ADVANCED_FACE('',(#590),#474,.F.);
#3207=ADVANCED_FACE('',(#591),#3120,.F.);
#3208=ADVANCED_FACE('',(#592),#475,.F.);
#3209=ADVANCED_FACE('',(#593),#3121,.T.);
#3210=ADVANCED_FACE('',(#594,#397,#398,#399,#400,#401),#476,.T.);
#3211=ADVANCED_FACE('',(#595),#3122,.F.);
#3212=ADVANCED_FACE('',(#596),#3123,.F.);
#3213=ADVANCED_FACE('',(#597),#3124,.F.);
#3214=ADVANCED_FACE('',(#598),#3125,.F.);
#3215=ADVANCED_FACE('',(#599),#3126,.F.);
#3216=ADVANCED_FACE('',(#600,#402),#477,.T.);
#3217=ADVANCED_FACE('',(#601,#403),#3127,.T.);
#3218=ADVANCED_FACE('',(#602,#404),#3128,.F.);
#3219=ADVANCED_FACE('',(#603,#405,#406,#407,#408,#409),#478,.T.);
#3220=ADVANCED_FACE('',(#604,#410,#411,#412,#413,#414),#479,.F.);
#3221=ADVANCED_FACE('',(#605),#480,.F.);
#3222=ADVANCED_FACE('',(#606),#481,.F.);
#3223=ADVANCED_FACE('',(#607),#482,.F.);
#3224=ADVANCED_FACE('',(#608),#483,.F.);
#3225=ADVANCED_FACE('',(#609),#484,.F.);
#3226=ADVANCED_FACE('',(#610),#485,.F.);
#3227=ADVANCED_FACE('',(#611),#486,.F.);
#3228=ADVANCED_FACE('',(#612),#487,.F.);
#3229=ADVANCED_FACE('',(#613),#488,.F.);
#3230=ADVANCED_FACE('',(#614),#489,.T.);
#3231=ADVANCED_FACE('',(#615),#265,.T.);
#3232=ADVANCED_FACE('',(#616),#3129,.T.);
#3233=ADVANCED_FACE('',(#617),#266,.T.);
#3234=ADVANCED_FACE('',(#618,#415),#490,.T.);
#3235=ADVANCED_FACE('',(#619),#267,.T.);
#3236=ADVANCED_FACE('',(#620),#3130,.T.);
#3237=ADVANCED_FACE('',(#621),#3131,.F.);
#3238=ADVANCED_FACE('',(#622),#491,.T.);
#3239=ADVANCED_FACE('',(#623),#3132,.F.);
#3240=ADVANCED_FACE('',(#624),#492,.T.);
#3241=ADVANCED_FACE('',(#625),#3133,.F.);
#3242=ADVANCED_FACE('',(#626),#493,.T.);
#3243=ADVANCED_FACE('',(#627),#3134,.F.);
#3244=ADVANCED_FACE('',(#628),#494,.T.);
#3245=ADVANCED_FACE('',(#629),#3135,.F.);
#3246=ADVANCED_FACE('',(#630,#416),#495,.T.);
#3247=ADVANCED_FACE('',(#631),#3136,.F.);
#3248=ADVANCED_FACE('',(#632,#417),#3137,.T.);
#3249=ADVANCED_FACE('',(#633,#418,#419,#420,#421,#422),#496,.T.);
#3250=ADVANCED_FACE('',(#634,#423),#497,.F.);
#3251=ADVANCED_FACE('',(#635),#498,.T.);
#3252=ADVANCED_FACE('',(#636),#499,.T.);
#3253=ADVANCED_FACE('',(#637),#500,.T.);
#3254=ADVANCED_FACE('',(#638),#3138,.T.);
#3255=ADVANCED_FACE('',(#639,#424),#501,.F.);
#3256=ADVANCED_FACE('',(#640,#425),#502,.F.);
#3257=ADVANCED_FACE('',(#641),#3139,.T.);
#3258=ADVANCED_FACE('',(#642),#3140,.T.);
#3259=ADVANCED_FACE('',(#643),#503,.F.);
#3260=ADVANCED_FACE('',(#644),#263,.F.);
#3261=ADVANCED_FACE('',(#645),#3141,.T.);
#3262=ADVANCED_FACE('',(#646),#3142,.F.);
#3263=ADVANCED_FACE('',(#647),#268,.F.);
#3264=ADVANCED_FACE('',(#648,#426),#504,.T.);
#3265=ADVANCED_FACE('',(#649),#3143,.T.);
#3266=ADVANCED_FACE('',(#650,#427),#505,.T.);
#3267=ADVANCED_FACE('',(#651),#269,.F.);
#3268=ADVANCED_FACE('',(#652),#264,.F.);
#3269=ADVANCED_FACE('',(#653),#3144,.F.);
#3270=ADVANCED_FACE('',(#654,#428),#506,.T.);
#3271=ADVANCED_FACE('',(#655),#270,.T.);
#3272=ADVANCED_FACE('',(#656),#3145,.T.);
#3273=ADVANCED_FACE('',(#657),#271,.T.);
#3274=ADVANCED_FACE('',(#658,#429),#507,.T.);
#3275=ADVANCED_FACE('',(#659),#3146,.F.);
#3276=ADVANCED_FACE('',(#660),#247,.T.);
#3277=ADVANCED_FACE('',(#661),#248,.T.);
#3278=ADVANCED_FACE('',(#662),#249,.T.);
#3279=ADVANCED_FACE('',(#663),#250,.T.);
#3280=ADVANCED_FACE('',(#664),#251,.T.);
#3281=ADVANCED_FACE('',(#665),#252,.T.);
#3282=ADVANCED_FACE('',(#666),#253,.T.);
#3283=ADVANCED_FACE('',(#667),#254,.T.);
#3284=ADVANCED_FACE('',(#668),#255,.F.);
#3285=ADVANCED_FACE('',(#669),#3147,.T.);
#3286=ADVANCED_FACE('',(#670),#508,.T.);
#3287=ADVANCED_FACE('',(#671),#256,.F.);
#3288=ADVANCED_FACE('',(#672),#509,.T.);
#3289=ADVANCED_FACE('',(#673),#257,.F.);
#3290=ADVANCED_FACE('',(#674),#510,.T.);
#3291=ADVANCED_FACE('',(#675),#258,.F.);
#3292=ADVANCED_FACE('',(#676),#511,.T.);
#3293=ADVANCED_FACE('',(#677),#259,.F.);
#3294=ADVANCED_FACE('',(#678),#512,.T.);
#3295=ADVANCED_FACE('',(#679),#260,.F.);
#3296=ADVANCED_FACE('',(#680),#513,.T.);
#3297=ADVANCED_FACE('',(#681),#261,.F.);
#3298=ADVANCED_FACE('',(#682),#3148,.F.);
#3299=ADVANCED_FACE('',(#683),#514,.T.);
#3300=ADVANCED_FACE('',(#684),#262,.F.);
#3301=ADVANCED_FACE('',(#685,#430),#515,.T.);
#3302=ADVANCED_FACE('',(#686),#516,.T.);
#3303=ADVANCED_FACE('',(#687,#431),#517,.T.);
#3304=ADVANCED_FACE('',(#688),#3149,.T.);
#3305=ADVANCED_FACE('',(#689,#432),#518,.T.);
#3306=ADVANCED_FACE('',(#690),#3150,.F.);
#3307=ADVANCED_FACE('',(#691,#433),#519,.T.);
#3308=ADVANCED_FACE('',(#692),#3151,.T.);
#3309=ADVANCED_FACE('',(#693,#434),#520,.T.);
#3310=ADVANCED_FACE('',(#694),#3152,.F.);
#3311=ADVANCED_FACE('',(#695),#3153,.F.);
#3312=ADVANCED_FACE('',(#696,#435),#521,.T.);
#3313=ADVANCED_FACE('',(#697),#3154,.F.);
#3314=ADVANCED_FACE('',(#698,#436),#522,.T.);
#3315=ADVANCED_FACE('',(#699),#3155,.F.);
#3316=ADVANCED_FACE('',(#700,#437),#523,.T.);
#3317=ADVANCED_FACE('',(#701),#3156,.F.);
#3318=ADVANCED_FACE('',(#702,#438),#524,.T.);
#3319=ADVANCED_FACE('',(#703),#3157,.F.);
#3320=ADVANCED_FACE('',(#704),#3158,.F.);
#3321=ADVANCED_FACE('',(#705),#3159,.F.);
#3322=ADVANCED_FACE('',(#706),#3160,.F.);
#3323=ADVANCED_FACE('',(#707),#3161,.T.);
#3324=ADVANCED_FACE('',(#708,#439),#525,.F.);
#3325=ADVANCED_FACE('',(#709),#3162,.F.);
#3326=ADVANCED_FACE('',(#710),#3163,.T.);
#3327=ADVANCED_FACE('',(#711,#440,#441,#442,#443,#444),#526,.T.);
#3328=ADVANCED_FACE('',(#712,#445,#446,#447,#448,#449),#527,.F.);
#3329=ADVANCED_FACE('',(#713),#528,.F.);
#3330=ADVANCED_FACE('',(#714),#529,.F.);
#3331=ADVANCED_FACE('',(#715),#530,.F.);
#3332=ADVANCED_FACE('',(#716),#531,.F.);
#3333=ADVANCED_FACE('',(#717),#532,.F.);
#3334=ADVANCED_FACE('',(#718),#533,.F.);
#3335=ADVANCED_FACE('',(#719),#534,.F.);
#3336=ADVANCED_FACE('',(#720),#535,.F.);
#3337=ADVANCED_FACE('',(#721),#536,.F.);
#3338=ADVANCED_FACE('',(#722),#537,.T.);
#3339=ADVANCED_FACE('',(#723),#272,.T.);
#3340=ADVANCED_FACE('',(#724),#3164,.T.);
#3341=ADVANCED_FACE('',(#725),#273,.T.);
#3342=ADVANCED_FACE('',(#726,#450),#538,.T.);
#3343=ADVANCED_FACE('',(#727),#274,.T.);
#3344=ADVANCED_FACE('',(#728),#3165,.T.);
#3345=ADVANCED_FACE('',(#729),#3166,.T.);
#3346=ADVANCED_FACE('',(#730),#539,.T.);
#3347=ADVANCED_FACE('',(#731,#451,#452),#540,.F.);
#3348=ADVANCED_FACE('',(#732,#453),#541,.F.);
#3349=ADVANCED_FACE('',(#733),#3167,.T.);
#3350=ADVANCED_FACE('',(#734),#3168,.T.);
#3351=ADVANCED_FACE('',(#735),#542,.F.);
#3352=ADVANCED_FACE('',(#736),#543,.T.);
#3353=ADVANCED_FACE('',(#737),#3169,.T.);
#3354=ADVANCED_FACE('',(#738,#454),#544,.F.);
#3355=ADVANCED_FACE('',(#739),#3170,.T.);
#3356=ADVANCED_FACE('',(#740),#3171,.T.);
#3357=ADVANCED_FACE('',(#741),#545,.T.);
#3358=ADVANCED_FACE('',(#742),#546,.F.);
#3359=ADVANCED_FACE('',(#743),#3172,.F.);
#3360=ADVANCED_FACE('',(#744),#3173,.T.);
#3361=ADVANCED_FACE('',(#745,#455),#547,.T.);
#3362=ADVANCED_FACE('',(#746,#456),#548,.F.);
#3363=ADVANCED_FACE('',(#747),#549,.T.);
#3364=ADVANCED_FACE('',(#748),#3174,.F.);
#3365=ADVANCED_FACE('',(#749),#550,.T.);
#3366=ADVANCED_FACE('',(#750,#457),#3175,.F.);
#3367=ADVANCED_FACE('',(#751,#458),#3176,.T.);
#3368=ADVANCED_FACE('',(#752,#459),#551,.T.);
#3369=ADVANCED_FACE('',(#753,#460),#552,.F.);
#3370=ADVANCED_FACE('',(#754),#553,.F.);
#3371=ADVANCED_FACE('',(#755),#554,.F.);
#3372=ADVANCED_FACE('',(#756),#555,.F.);
#3373=ADVANCED_FACE('',(#757),#556,.F.);
#3374=ADVANCED_FACE('',(#758),#557,.F.);
#3375=ADVANCED_FACE('',(#759),#558,.F.);
#3376=ADVANCED_FACE('',(#760),#559,.F.);
#3377=ADVANCED_FACE('',(#761),#560,.F.);
#3378=ADVANCED_FACE('',(#762,#461),#561,.T.);
#3379=ADVANCED_FACE('',(#763),#275,.T.);
#3380=ADVANCED_FACE('',(#764),#3177,.T.);
#3381=CLOSED_SHELL('',(#3178,#3179,#3180,#3181,#3182,#3183,#3184,#3185,
#3186,#3187,#3188,#3189,#3190,#3191));
#3382=CLOSED_SHELL('',(#3192,#3193,#3194,#3195,#3196,#3197,#3198,#3199,
#3200,#3201,#3202,#3203,#3204,#3205,#3206,#3207,#3208,#3209,#3210,#3211,
#3212,#3213,#3214,#3215,#3216,#3217,#3218,#3219,#3220));
#3383=CLOSED_SHELL('',(#3221,#3222,#3223,#3224,#3225,#3226,#3227,#3228));
#3384=CLOSED_SHELL('',(#3229,#3230,#3231,#3232,#3233,#3234,#3235,#3236));
#3385=CLOSED_SHELL('',(#3237,#3238,#3239,#3240,#3241,#3242,#3243,#3244,
#3245,#3246,#3247,#3248,#3249,#3250,#3251,#3252,#3253,#3254,#3255,#3256,
#3257,#3258,#3259));
#3386=CLOSED_SHELL('',(#3260,#3261,#3262,#3263,#3264,#3265,#3266,#3267));
#3387=CLOSED_SHELL('',(#3268,#3269,#3270,#3271,#3272,#3273,#3274,#3275));
#3388=CLOSED_SHELL('',(#3276));
#3389=CLOSED_SHELL('',(#3277));
#3390=CLOSED_SHELL('',(#3278));
#3391=CLOSED_SHELL('',(#3279));
#3392=CLOSED_SHELL('',(#3280));
#3393=CLOSED_SHELL('',(#3281));
#3394=CLOSED_SHELL('',(#3282));
#3395=CLOSED_SHELL('',(#3283));
#3396=CLOSED_SHELL('',(#3284,#3285,#3286,#3287,#3288,#3289,#3290,#3291,
#3292,#3293,#3294,#3295,#3296,#3297,#3298,#3299,#3300,#3301,#3302));
#3397=CLOSED_SHELL('',(#3303,#3304,#3305,#3306));
#3398=CLOSED_SHELL('',(#3307,#3308,#3309,#3310));
#3399=CLOSED_SHELL('',(#3311,#3312,#3313,#3314,#3315,#3316,#3317,#3318,
#3319,#3320,#3321,#3322,#3323,#3324,#3325,#3326,#3327,#3328));
#3400=CLOSED_SHELL('',(#3329,#3330,#3331,#3332,#3333,#3334,#3335,#3336));
#3401=CLOSED_SHELL('',(#3337,#3338,#3339,#3340,#3341,#3342,#3343,#3344));
#3402=CLOSED_SHELL('',(#3345,#3346,#3347,#3348,#3349,#3350,#3351,#3352,
#3353,#3354,#3355,#3356,#3357,#3358));
#3403=CLOSED_SHELL('',(#3359,#3360,#3361,#3362));
#3404=CLOSED_SHELL('',(#3363,#3364,#3365,#3366,#3367,#3368,#3369));
#3405=CLOSED_SHELL('',(#3370,#3371,#3372,#3373,#3374,#3375,#3376,#3377,
#3378,#3379,#3380));
#3406=DERIVED_UNIT_ELEMENT(#3436,1.);
#3407=DERIVED_UNIT_ELEMENT(#6707,-3.);
#3408=DERIVED_UNIT_ELEMENT(#3436,1.);
#3409=DERIVED_UNIT_ELEMENT(#6707,-3.);
#3410=DERIVED_UNIT_ELEMENT(#3436,1.);
#3411=DERIVED_UNIT_ELEMENT(#6707,-3.);
#3412=DERIVED_UNIT_ELEMENT(#3436,1.);
#3413=DERIVED_UNIT_ELEMENT(#6707,-3.);
#3414=DERIVED_UNIT_ELEMENT(#3436,1.);
#3415=DERIVED_UNIT_ELEMENT(#6707,-3.);
#3416=DERIVED_UNIT_ELEMENT(#3436,1.);
#3417=DERIVED_UNIT_ELEMENT(#6707,-3.);
#3418=DERIVED_UNIT_ELEMENT(#3436,1.);
#3419=DERIVED_UNIT_ELEMENT(#6707,-3.);
#3420=DERIVED_UNIT_ELEMENT(#3436,1.);
#3421=DERIVED_UNIT_ELEMENT(#6707,-3.);
#3422=DERIVED_UNIT_ELEMENT(#3436,1.);
#3423=DERIVED_UNIT_ELEMENT(#6707,-3.);
#3424=DERIVED_UNIT_ELEMENT(#3436,1.);
#3425=DERIVED_UNIT_ELEMENT(#6707,-3.);
#3426=DERIVED_UNIT_ELEMENT(#3436,1.);
#3427=DERIVED_UNIT_ELEMENT(#6707,-3.);
#3428=DERIVED_UNIT_ELEMENT(#3436,1.);
#3429=DERIVED_UNIT_ELEMENT(#6707,-3.);
#3430=DERIVED_UNIT_ELEMENT(#3436,1.);
#3431=DERIVED_UNIT_ELEMENT(#6707,-3.);
#3432=DERIVED_UNIT_ELEMENT(#3436,1.);
#3433=DERIVED_UNIT_ELEMENT(#6707,-3.);
#3434=DERIVED_UNIT_ELEMENT(#3436,1.);
#3435=DERIVED_UNIT_ELEMENT(#6707,-3.);
#3436=(
MASS_UNIT()
NAMED_UNIT(*)
SI_UNIT(.KILO.,.GRAM.)
);
#3437=DERIVED_UNIT((#3406,#3407));
#3438=DERIVED_UNIT((#3408,#3409));
#3439=DERIVED_UNIT((#3410,#3411));
#3440=DERIVED_UNIT((#3412,#3413));
#3441=DERIVED_UNIT((#3414,#3415));
#3442=DERIVED_UNIT((#3416,#3417));
#3443=DERIVED_UNIT((#3418,#3419));
#3444=DERIVED_UNIT((#3420,#3421));
#3445=DERIVED_UNIT((#3422,#3423));
#3446=DERIVED_UNIT((#3424,#3425));
#3447=DERIVED_UNIT((#3426,#3427));
#3448=DERIVED_UNIT((#3428,#3429));
#3449=DERIVED_UNIT((#3430,#3431));
#3450=DERIVED_UNIT((#3432,#3433));
#3451=DERIVED_UNIT((#3434,#3435));
#3452=MEASURE_REPRESENTATION_ITEM('density measure',
POSITIVE_RATIO_MEASURE(7850.),#3437);
#3453=MEASURE_REPRESENTATION_ITEM('density measure',
POSITIVE_RATIO_MEASURE(7850.),#3438);
#3454=MEASURE_REPRESENTATION_ITEM('density measure',
POSITIVE_RATIO_MEASURE(7850.),#3439);
#3455=MEASURE_REPRESENTATION_ITEM('density measure',
POSITIVE_RATIO_MEASURE(7850.),#3440);
#3456=MEASURE_REPRESENTATION_ITEM('density measure',
POSITIVE_RATIO_MEASURE(7850.),#3441);
#3457=MEASURE_REPRESENTATION_ITEM('density measure',
POSITIVE_RATIO_MEASURE(7850.),#3442);
#3458=MEASURE_REPRESENTATION_ITEM('density measure',
POSITIVE_RATIO_MEASURE(7850.),#3443);
#3459=MEASURE_REPRESENTATION_ITEM('density measure',
POSITIVE_RATIO_MEASURE(7850.),#3444);
#3460=MEASURE_REPRESENTATION_ITEM('density measure',
POSITIVE_RATIO_MEASURE(7850.),#3445);
#3461=MEASURE_REPRESENTATION_ITEM('density measure',
POSITIVE_RATIO_MEASURE(7850.),#3446);
#3462=MEASURE_REPRESENTATION_ITEM('density measure',
POSITIVE_RATIO_MEASURE(7850.),#3447);
#3463=MEASURE_REPRESENTATION_ITEM('density measure',
POSITIVE_RATIO_MEASURE(7850.),#3448);
#3464=MEASURE_REPRESENTATION_ITEM('density measure',
POSITIVE_RATIO_MEASURE(7850.),#3449);
#3465=MEASURE_REPRESENTATION_ITEM('density measure',
POSITIVE_RATIO_MEASURE(7850.),#3450);
#3466=MEASURE_REPRESENTATION_ITEM('density measure',
POSITIVE_RATIO_MEASURE(7850.),#3451);
#3467=PROPERTY_DEFINITION_REPRESENTATION(#3542,#3497);
#3468=PROPERTY_DEFINITION_REPRESENTATION(#3543,#3498);
#3469=PROPERTY_DEFINITION_REPRESENTATION(#3544,#3499);
#3470=PROPERTY_DEFINITION_REPRESENTATION(#3545,#3500);
#3471=PROPERTY_DEFINITION_REPRESENTATION(#3546,#3501);
#3472=PROPERTY_DEFINITION_REPRESENTATION(#3547,#3502);
#3473=PROPERTY_DEFINITION_REPRESENTATION(#3548,#3503);
#3474=PROPERTY_DEFINITION_REPRESENTATION(#3549,#3504);
#3475=PROPERTY_DEFINITION_REPRESENTATION(#3550,#3505);
#3476=PROPERTY_DEFINITION_REPRESENTATION(#3551,#3506);
#3477=PROPERTY_DEFINITION_REPRESENTATION(#3552,#3507);
#3478=PROPERTY_DEFINITION_REPRESENTATION(#3553,#3508);
#3479=PROPERTY_DEFINITION_REPRESENTATION(#3554,#3509);
#3480=PROPERTY_DEFINITION_REPRESENTATION(#3555,#3510);
#3481=PROPERTY_DEFINITION_REPRESENTATION(#3556,#3511);
#3482=PROPERTY_DEFINITION_REPRESENTATION(#3557,#3512);
#3483=PROPERTY_DEFINITION_REPRESENTATION(#3558,#3513);
#3484=PROPERTY_DEFINITION_REPRESENTATION(#3559,#3514);
#3485=PROPERTY_DEFINITION_REPRESENTATION(#3560,#3515);
#3486=PROPERTY_DEFINITION_REPRESENTATION(#3561,#3516);
#3487=PROPERTY_DEFINITION_REPRESENTATION(#3562,#3517);
#3488=PROPERTY_DEFINITION_REPRESENTATION(#3563,#3518);
#3489=PROPERTY_DEFINITION_REPRESENTATION(#3564,#3519);
#3490=PROPERTY_DEFINITION_REPRESENTATION(#3565,#3520);
#3491=PROPERTY_DEFINITION_REPRESENTATION(#3566,#3521);
#3492=PROPERTY_DEFINITION_REPRESENTATION(#3567,#3522);
#3493=PROPERTY_DEFINITION_REPRESENTATION(#3568,#3523);
#3494=PROPERTY_DEFINITION_REPRESENTATION(#3569,#3524);
#3495=PROPERTY_DEFINITION_REPRESENTATION(#3570,#3525);
#3496=PROPERTY_DEFINITION_REPRESENTATION(#3571,#3526);
#3497=REPRESENTATION('material name',(#3527),#6686);
#3498=REPRESENTATION('density',(#3452),#6686);
#3499=REPRESENTATION('material name',(#3528),#6687);
#3500=REPRESENTATION('density',(#3453),#6687);
#3501=REPRESENTATION('material name',(#3529),#6688);
#3502=REPRESENTATION('density',(#3454),#6688);
#3503=REPRESENTATION('material name',(#3530),#6691);
#3504=REPRESENTATION('density',(#3455),#6691);
#3505=REPRESENTATION('material name',(#3531),#6693);
#3506=REPRESENTATION('density',(#3456),#6693);
#3507=REPRESENTATION('material name',(#3532),#6694);
#3508=REPRESENTATION('density',(#3457),#6694);
#3509=REPRESENTATION('material name',(#3533),#6695);
#3510=REPRESENTATION('density',(#3458),#6695);
#3511=REPRESENTATION('material name',(#3534),#6696);
#3512=REPRESENTATION('density',(#3459),#6696);
#3513=REPRESENTATION('material name',(#3535),#6697);
#3514=REPRESENTATION('density',(#3460),#6697);
#3515=REPRESENTATION('material name',(#3536),#6698);
#3516=REPRESENTATION('density',(#3461),#6698);
#3517=REPRESENTATION('material name',(#3537),#6699);
#3518=REPRESENTATION('density',(#3462),#6699);
#3519=REPRESENTATION('material name',(#3538),#6701);
#3520=REPRESENTATION('density',(#3463),#6701);
#3521=REPRESENTATION('material name',(#3539),#6702);
#3522=REPRESENTATION('density',(#3464),#6702);
#3523=REPRESENTATION('material name',(#3540),#6703);
#3524=REPRESENTATION('density',(#3465),#6703);
#3525=REPRESENTATION('material name',(#3541),#6704);
#3526=REPRESENTATION('density',(#3466),#6704);
#3527=DESCRIPTIVE_REPRESENTATION_ITEM('Steel','Steel');
#3528=DESCRIPTIVE_REPRESENTATION_ITEM('Steel','Steel');
#3529=DESCRIPTIVE_REPRESENTATION_ITEM('Steel','Steel');
#3530=DESCRIPTIVE_REPRESENTATION_ITEM('Steel','Steel');
#3531=DESCRIPTIVE_REPRESENTATION_ITEM('Steel','Steel');
#3532=DESCRIPTIVE_REPRESENTATION_ITEM('Steel','Steel');
#3533=DESCRIPTIVE_REPRESENTATION_ITEM('Steel','Steel');
#3534=DESCRIPTIVE_REPRESENTATION_ITEM('Steel','Steel');
#3535=DESCRIPTIVE_REPRESENTATION_ITEM('Steel','Steel');
#3536=DESCRIPTIVE_REPRESENTATION_ITEM('Steel','Steel');
#3537=DESCRIPTIVE_REPRESENTATION_ITEM('Steel','Steel');
#3538=DESCRIPTIVE_REPRESENTATION_ITEM('Steel','Steel');
#3539=DESCRIPTIVE_REPRESENTATION_ITEM('Steel','Steel');
#3540=DESCRIPTIVE_REPRESENTATION_ITEM('Steel','Steel');
#3541=DESCRIPTIVE_REPRESENTATION_ITEM('Steel','Steel');
#3542=PROPERTY_DEFINITION('material property','material name',#6835);
#3543=PROPERTY_DEFINITION('material property','density of part',#6835);
#3544=PROPERTY_DEFINITION('material property','material name',#6836);
#3545=PROPERTY_DEFINITION('material property','density of part',#6836);
#3546=PROPERTY_DEFINITION('material property','material name',#6837);
#3547=PROPERTY_DEFINITION('material property','density of part',#6837);
#3548=PROPERTY_DEFINITION('material property','material name',#6840);
#3549=PROPERTY_DEFINITION('material property','density of part',#6840);
#3550=PROPERTY_DEFINITION('material property','material name',#6842);
#3551=PROPERTY_DEFINITION('material property','density of part',#6842);
#3552=PROPERTY_DEFINITION('material property','material name',#6843);
#3553=PROPERTY_DEFINITION('material property','density of part',#6843);
#3554=PROPERTY_DEFINITION('material property','material name',#6844);
#3555=PROPERTY_DEFINITION('material property','density of part',#6844);
#3556=PROPERTY_DEFINITION('material property','material name',#6845);
#3557=PROPERTY_DEFINITION('material property','density of part',#6845);
#3558=PROPERTY_DEFINITION('material property','material name',#6846);
#3559=PROPERTY_DEFINITION('material property','density of part',#6846);
#3560=PROPERTY_DEFINITION('material property','material name',#6847);
#3561=PROPERTY_DEFINITION('material property','density of part',#6847);
#3562=PROPERTY_DEFINITION('material property','material name',#6848);
#3563=PROPERTY_DEFINITION('material property','density of part',#6848);
#3564=PROPERTY_DEFINITION('material property','material name',#6850);
#3565=PROPERTY_DEFINITION('material property','density of part',#6850);
#3566=PROPERTY_DEFINITION('material property','material name',#6851);
#3567=PROPERTY_DEFINITION('material property','density of part',#6851);
#3568=PROPERTY_DEFINITION('material property','material name',#6852);
#3569=PROPERTY_DEFINITION('material property','density of part',#6852);
#3570=PROPERTY_DEFINITION('material property','material name',#6853);
#3571=PROPERTY_DEFINITION('material property','density of part',#6853);
#3572=AXIS2_PLACEMENT_3D('',#5224,#4066,#4067);
#3573=AXIS2_PLACEMENT_3D('',#5225,#4068,#4069);
#3574=AXIS2_PLACEMENT_3D('',#5226,#4070,#4071);
#3575=AXIS2_PLACEMENT_3D('',#5227,#4072,#4073);
#3576=AXIS2_PLACEMENT_3D('',#5229,#4074,#4075);
#3577=AXIS2_PLACEMENT_3D('',#5232,#4077,#4078);
#3578=AXIS2_PLACEMENT_3D('',#5233,#4079,#4080);
#3579=AXIS2_PLACEMENT_3D('',#5235,#4081,#4082);
#3580=AXIS2_PLACEMENT_3D('',#5238,#4084,#4085);
#3581=AXIS2_PLACEMENT_3D('',#5239,#4086,#4087);
#3582=AXIS2_PLACEMENT_3D('',#5241,#4088,#4089);
#3583=AXIS2_PLACEMENT_3D('',#5244,#4091,#4092);
#3584=AXIS2_PLACEMENT_3D('',#5245,#4093,#4094);
#3585=AXIS2_PLACEMENT_3D('',#5247,#4095,#4096);
#3586=AXIS2_PLACEMENT_3D('',#5250,#4098,#4099);
#3587=AXIS2_PLACEMENT_3D('',#5251,#4100,#4101);
#3588=AXIS2_PLACEMENT_3D('',#5253,#4102,#4103);
#3589=AXIS2_PLACEMENT_3D('',#5256,#4105,#4106);
#3590=AXIS2_PLACEMENT_3D('',#5257,#4107,#4108);
#3591=AXIS2_PLACEMENT_3D('',#5259,#4109,#4110);
#3592=AXIS2_PLACEMENT_3D('',#5262,#4112,#4113);
#3593=AXIS2_PLACEMENT_3D('',#5263,#4114,#4115);
#3594=AXIS2_PLACEMENT_3D('',#5265,#4116,#4117);
#3595=AXIS2_PLACEMENT_3D('',#5268,#4119,#4120);
#3596=AXIS2_PLACEMENT_3D('',#5269,#4121,#4122);
#3597=AXIS2_PLACEMENT_3D('',#5271,#4123,#4124);
#3598=AXIS2_PLACEMENT_3D('',#5274,#4126,#4127);
#3599=AXIS2_PLACEMENT_3D('',#5275,#4128,#4129);
#3600=AXIS2_PLACEMENT_3D('',#5284,#4134,#4135);
#3601=AXIS2_PLACEMENT_3D('',#5290,#4139,#4140);
#3602=AXIS2_PLACEMENT_3D('',#5296,#4144,#4145);
#3603=AXIS2_PLACEMENT_3D('',#5299,#4148,#4149);
#3604=AXIS2_PLACEMENT_3D('',#5300,#4150,#4151);
#3605=AXIS2_PLACEMENT_3D('',#5301,#4152,#4153);
#3606=AXIS2_PLACEMENT_3D('',#5302,#4154,#4155);
#3607=AXIS2_PLACEMENT_3D('',#5380,#4157,#4158);
#3608=AXIS2_PLACEMENT_3D('',#5382,#4159,#4160);
#3609=AXIS2_PLACEMENT_3D('',#5385,#4162,#4163);
#3610=AXIS2_PLACEMENT_3D('',#5386,#4164,#4165);
#3611=AXIS2_PLACEMENT_3D('',#5387,#4166,#4167);
#3612=AXIS2_PLACEMENT_3D('',#5389,#4168,#4169);
#3613=AXIS2_PLACEMENT_3D('',#5392,#4171,#4172);
#3614=AXIS2_PLACEMENT_3D('',#5393,#4173,#4174);
#3615=AXIS2_PLACEMENT_3D('',#5394,#4175,#4176);
#3616=AXIS2_PLACEMENT_3D('',#5396,#4177,#4178);
#3617=AXIS2_PLACEMENT_3D('',#5399,#4180,#4181);
#3618=AXIS2_PLACEMENT_3D('',#5400,#4182,#4183);
#3619=AXIS2_PLACEMENT_3D('',#5401,#4184,#4185);
#3620=AXIS2_PLACEMENT_3D('',#5403,#4186,#4187);
#3621=AXIS2_PLACEMENT_3D('',#5406,#4189,#4190);
#3622=AXIS2_PLACEMENT_3D('',#5407,#4191,#4192);
#3623=AXIS2_PLACEMENT_3D('',#5408,#4193,#4194);
#3624=AXIS2_PLACEMENT_3D('',#5411,#4195,#4196);
#3625=AXIS2_PLACEMENT_3D('',#5412,#4197,#4198);
#3626=AXIS2_PLACEMENT_3D('',#5413,#4199,#4200);
#3627=AXIS2_PLACEMENT_3D('',#5417,#4202,#4203);
#3628=AXIS2_PLACEMENT_3D('',#5419,#4205,#4206);
#3629=AXIS2_PLACEMENT_3D('',#5424,#4208,#4209);
#3630=AXIS2_PLACEMENT_3D('',#5427,#4211,#4212);
#3631=AXIS2_PLACEMENT_3D('',#5428,#4213,#4214);
#3632=AXIS2_PLACEMENT_3D('',#5429,#4215,#4216);
#3633=AXIS2_PLACEMENT_3D('',#5430,#4217,#4218);
#3634=AXIS2_PLACEMENT_3D('',#5435,#4220,#4221);
#3635=AXIS2_PLACEMENT_3D('',#5438,#4223,#4224);
#3636=AXIS2_PLACEMENT_3D('',#5439,#4225,#4226);
#3637=AXIS2_PLACEMENT_3D('',#5440,#4227,#4228);
#3638=AXIS2_PLACEMENT_3D('',#5441,#4229,#4230);
#3639=AXIS2_PLACEMENT_3D('',#5446,#4232,#4233);
#3640=AXIS2_PLACEMENT_3D('',#5449,#4235,#4236);
#3641=AXIS2_PLACEMENT_3D('',#5450,#4237,#4238);
#3642=AXIS2_PLACEMENT_3D('',#5451,#4239,#4240);
#3643=AXIS2_PLACEMENT_3D('',#5452,#4241,#4242);
#3644=AXIS2_PLACEMENT_3D('',#5454,#4243,#4244);
#3645=AXIS2_PLACEMENT_3D('',#5457,#4246,#4247);
#3646=AXIS2_PLACEMENT_3D('',#5458,#4248,#4249);
#3647=AXIS2_PLACEMENT_3D('',#5459,#4250,#4251);
#3648=AXIS2_PLACEMENT_3D('',#5460,#4252,#4253);
#3649=AXIS2_PLACEMENT_3D('',#5461,#4254,#4255);
#3650=AXIS2_PLACEMENT_3D('',#5462,#4256,#4257);
#3651=AXIS2_PLACEMENT_3D('',#5464,#4258,#4259);
#3652=AXIS2_PLACEMENT_3D('',#5466,#4260,#4261);
#3653=AXIS2_PLACEMENT_3D('',#5468,#4262,#4263);
#3654=AXIS2_PLACEMENT_3D('',#5470,#4264,#4265);
#3655=AXIS2_PLACEMENT_3D('',#5472,#4266,#4267);
#3656=AXIS2_PLACEMENT_3D('',#5473,#4268,#4269);
#3657=AXIS2_PLACEMENT_3D('',#5475,#4270,#4271);
#3658=AXIS2_PLACEMENT_3D('',#5477,#4273,#4274);
#3659=AXIS2_PLACEMENT_3D('',#5479,#4275,#4276);
#3660=AXIS2_PLACEMENT_3D('',#5481,#4278,#4279);
#3661=AXIS2_PLACEMENT_3D('',#5483,#4280,#4281);
#3662=AXIS2_PLACEMENT_3D('',#5485,#4283,#4284);
#3663=AXIS2_PLACEMENT_3D('',#5487,#4285,#4286);
#3664=AXIS2_PLACEMENT_3D('',#5489,#4288,#4289);
#3665=AXIS2_PLACEMENT_3D('',#5491,#4290,#4291);
#3666=AXIS2_PLACEMENT_3D('',#5494,#4293,#4294);
#3667=AXIS2_PLACEMENT_3D('',#5495,#4295,#4296);
#3668=AXIS2_PLACEMENT_3D('',#5497,#4297,#4298);
#3669=AXIS2_PLACEMENT_3D('',#5498,#4299,#4300);
#3670=AXIS2_PLACEMENT_3D('',#5501,#4302,#4303);
#3671=AXIS2_PLACEMENT_3D('',#5502,#4304,#4305);
#3672=AXIS2_PLACEMENT_3D('',#5505,#4307,#4308);
#3673=AXIS2_PLACEMENT_3D('',#5506,#4309,#4310);
#3674=AXIS2_PLACEMENT_3D('',#5507,#4311,#4312);
#3675=AXIS2_PLACEMENT_3D('',#5508,#4313,#4314);
#3676=AXIS2_PLACEMENT_3D('',#5509,#4315,#4316);
#3677=AXIS2_PLACEMENT_3D('',#5518,#4321,#4322);
#3678=AXIS2_PLACEMENT_3D('',#5524,#4326,#4327);
#3679=AXIS2_PLACEMENT_3D('',#5530,#4331,#4332);
#3680=AXIS2_PLACEMENT_3D('',#5536,#4336,#4337);
#3681=AXIS2_PLACEMENT_3D('',#5542,#4341,#4342);
#3682=AXIS2_PLACEMENT_3D('',#5545,#4345,#4346);
#3683=AXIS2_PLACEMENT_3D('',#5546,#4347,#4348);
#3684=AXIS2_PLACEMENT_3D('',#5547,#4349,#4350);
#3685=AXIS2_PLACEMENT_3D('',#5549,#4351,#4352);
#3686=AXIS2_PLACEMENT_3D('',#5550,#4353,#4354);
#3687=AXIS2_PLACEMENT_3D('',#5552,#4355,#4356);
#3688=AXIS2_PLACEMENT_3D('',#5553,#4357,#4358);
#3689=AXIS2_PLACEMENT_3D('',#5555,#4359,#4360);
#3690=AXIS2_PLACEMENT_3D('',#5557,#4362,#4363);
#3691=AXIS2_PLACEMENT_3D('',#5559,#4364,#4365);
#3692=AXIS2_PLACEMENT_3D('',#5561,#4367,#4368);
#3693=AXIS2_PLACEMENT_3D('',#5563,#4369,#4370);
#3694=AXIS2_PLACEMENT_3D('',#5565,#4372,#4373);
#3695=AXIS2_PLACEMENT_3D('',#5567,#4374,#4375);
#3696=AXIS2_PLACEMENT_3D('',#5568,#4376,#4377);
#3697=AXIS2_PLACEMENT_3D('',#5570,#4378,#4379);
#3698=AXIS2_PLACEMENT_3D('',#5572,#4381,#4382);
#3699=AXIS2_PLACEMENT_3D('',#5574,#4384,#4385);
#3700=AXIS2_PLACEMENT_3D('',#5575,#4386,#4387);
#3701=AXIS2_PLACEMENT_3D('',#5576,#4388,#4389);
#3702=AXIS2_PLACEMENT_3D('',#5577,#4390,#4391);
#3703=AXIS2_PLACEMENT_3D('',#5579,#4392,#4393);
#3704=AXIS2_PLACEMENT_3D('',#5582,#4395,#4396);
#3705=AXIS2_PLACEMENT_3D('',#5583,#4397,#4398);
#3706=AXIS2_PLACEMENT_3D('',#5584,#4399,#4400);
#3707=AXIS2_PLACEMENT_3D('',#5586,#4401,#4402);
#3708=AXIS2_PLACEMENT_3D('',#5589,#4404,#4405);
#3709=AXIS2_PLACEMENT_3D('',#5590,#4406,#4407);
#3710=AXIS2_PLACEMENT_3D('',#5591,#4408,#4409);
#3711=AXIS2_PLACEMENT_3D('',#5593,#4410,#4411);
#3712=AXIS2_PLACEMENT_3D('',#5596,#4413,#4414);
#3713=AXIS2_PLACEMENT_3D('',#5597,#4415,#4416);
#3714=AXIS2_PLACEMENT_3D('',#5598,#4417,#4418);
#3715=AXIS2_PLACEMENT_3D('',#5600,#4419,#4420);
#3716=AXIS2_PLACEMENT_3D('',#5603,#4422,#4423);
#3717=AXIS2_PLACEMENT_3D('',#5604,#4424,#4425);
#3718=AXIS2_PLACEMENT_3D('',#5605,#4426,#4427);
#3719=AXIS2_PLACEMENT_3D('',#5607,#4428,#4429);
#3720=AXIS2_PLACEMENT_3D('',#5610,#4431,#4432);
#3721=AXIS2_PLACEMENT_3D('',#5611,#4433,#4434);
#3722=AXIS2_PLACEMENT_3D('',#5613,#4435,#4436);
#3723=AXIS2_PLACEMENT_3D('',#5614,#4437,#4438);
#3724=AXIS2_PLACEMENT_3D('',#5616,#4439,#4440);
#3725=AXIS2_PLACEMENT_3D('',#5618,#4442,#4443);
#3726=AXIS2_PLACEMENT_3D('',#5620,#4444,#4445);
#3727=AXIS2_PLACEMENT_3D('',#5623,#4447,#4448);
#3728=AXIS2_PLACEMENT_3D('',#5628,#4450,#4451);
#3729=AXIS2_PLACEMENT_3D('',#5631,#4453,#4454);
#3730=AXIS2_PLACEMENT_3D('',#5632,#4455,#4456);
#3731=AXIS2_PLACEMENT_3D('',#5633,#4457,#4458);
#3732=AXIS2_PLACEMENT_3D('',#5634,#4459,#4460);
#3733=AXIS2_PLACEMENT_3D('',#5640,#4464,#4465);
#3734=AXIS2_PLACEMENT_3D('',#5643,#4467,#4468);
#3735=AXIS2_PLACEMENT_3D('',#5644,#4469,#4470);
#3736=AXIS2_PLACEMENT_3D('',#5648,#4473,#4474);
#3737=AXIS2_PLACEMENT_3D('',#5649,#4475,#4476);
#3738=AXIS2_PLACEMENT_3D('',#5650,#4477,#4478);
#3739=AXIS2_PLACEMENT_3D('',#5652,#4479,#4480);
#3740=AXIS2_PLACEMENT_3D('',#5653,#4481,#4482);
#3741=AXIS2_PLACEMENT_3D('',#5655,#4483,#4484);
#3742=AXIS2_PLACEMENT_3D('',#5657,#4485,#4486);
#3743=AXIS2_PLACEMENT_3D('',#5658,#4487,#4488);
#3744=AXIS2_PLACEMENT_3D('',#5660,#4490,#4491);
#3745=AXIS2_PLACEMENT_3D('',#5663,#4493,#4494);
#3746=AXIS2_PLACEMENT_3D('',#5664,#4495,#4496);
#3747=AXIS2_PLACEMENT_3D('',#5665,#4497,#4498);
#3748=AXIS2_PLACEMENT_3D('',#5666,#4499,#4500);
#3749=AXIS2_PLACEMENT_3D('',#5667,#4501,#4502);
#3750=AXIS2_PLACEMENT_3D('',#5670,#4503,#4504);
#3751=AXIS2_PLACEMENT_3D('',#5671,#4505,#4506);
#3752=AXIS2_PLACEMENT_3D('',#5673,#4507,#4508);
#3753=AXIS2_PLACEMENT_3D('',#5675,#4509,#4510);
#3754=AXIS2_PLACEMENT_3D('',#5676,#4511,#4512);
#3755=AXIS2_PLACEMENT_3D('',#5677,#4513,#4514);
#3756=AXIS2_PLACEMENT_3D('',#5680,#4516,#4517);
#3757=AXIS2_PLACEMENT_3D('',#5681,#4518,#4519);
#3758=AXIS2_PLACEMENT_3D('',#5683,#4520,#4521);
#3759=AXIS2_PLACEMENT_3D('',#5686,#4523,#4524);
#3760=AXIS2_PLACEMENT_3D('',#5687,#4525,#4526);
#3761=AXIS2_PLACEMENT_3D('',#5690,#4528,#4529);
#3762=AXIS2_PLACEMENT_3D('',#5691,#4530,#4531);
#3763=AXIS2_PLACEMENT_3D('',#5692,#4532,#4533);
#3764=AXIS2_PLACEMENT_3D('',#5694,#4534,#4535);
#3765=AXIS2_PLACEMENT_3D('',#5696,#4537,#4538);
#3766=AXIS2_PLACEMENT_3D('',#5698,#4539,#4540);
#3767=AXIS2_PLACEMENT_3D('',#5699,#4541,#4542);
#3768=AXIS2_PLACEMENT_3D('',#5701,#4544,#4545);
#3769=AXIS2_PLACEMENT_3D('',#5702,#4546,#4547);
#3770=AXIS2_PLACEMENT_3D('',#5705,#4548,#4549);
#3771=AXIS2_PLACEMENT_3D('',#5706,#4550,#4551);
#3772=AXIS2_PLACEMENT_3D('',#5708,#4552,#4553);
#3773=AXIS2_PLACEMENT_3D('',#5710,#4554,#4555);
#3774=AXIS2_PLACEMENT_3D('',#5711,#4556,#4557);
#3775=AXIS2_PLACEMENT_3D('',#5712,#4558,#4559);
#3776=AXIS2_PLACEMENT_3D('',#5714,#4560,#4561);
#3777=AXIS2_PLACEMENT_3D('',#5716,#4563,#4564);
#3778=AXIS2_PLACEMENT_3D('',#5718,#4565,#4566);
#3779=AXIS2_PLACEMENT_3D('',#5720,#4567,#4568);
#3780=AXIS2_PLACEMENT_3D('',#5721,#4569,#4570);
#3781=AXIS2_PLACEMENT_3D('',#5723,#4571,#4572);
#3782=AXIS2_PLACEMENT_3D('',#5725,#4574,#4575);
#3783=AXIS2_PLACEMENT_3D('',#5727,#4576,#4577);
#3784=AXIS2_PLACEMENT_3D('',#5729,#4579,#4580);
#3785=AXIS2_PLACEMENT_3D('',#5731,#4581,#4582);
#3786=AXIS2_PLACEMENT_3D('',#5733,#4584,#4585);
#3787=AXIS2_PLACEMENT_3D('',#5734,#4586,#4587);
#3788=AXIS2_PLACEMENT_3D('',#5736,#4589,#4590);
#3789=AXIS2_PLACEMENT_3D('',#5737,#4591,#4592);
#3790=AXIS2_PLACEMENT_3D('',#5740,#4593,#4594);
#3791=AXIS2_PLACEMENT_3D('',#5741,#4595,#4596);
#3792=AXIS2_PLACEMENT_3D('',#5744,#4597,#4598);
#3793=AXIS2_PLACEMENT_3D('',#5745,#4599,#4600);
#3794=AXIS2_PLACEMENT_3D('',#5748,#4601,#4602);
#3795=AXIS2_PLACEMENT_3D('',#5749,#4603,#4604);
#3796=AXIS2_PLACEMENT_3D('',#5752,#4605,#4606);
#3797=AXIS2_PLACEMENT_3D('',#5753,#4607,#4608);
#3798=AXIS2_PLACEMENT_3D('',#5756,#4609,#4610);
#3799=AXIS2_PLACEMENT_3D('',#5757,#4611,#4612);
#3800=AXIS2_PLACEMENT_3D('',#5760,#4613,#4614);
#3801=AXIS2_PLACEMENT_3D('',#5761,#4615,#4616);
#3802=AXIS2_PLACEMENT_3D('',#5764,#4617,#4618);
#3803=AXIS2_PLACEMENT_3D('',#5765,#4619,#4620);
#3804=AXIS2_PLACEMENT_3D('',#5768,#4621,#4622);
#3805=AXIS2_PLACEMENT_3D('',#5769,#4623,#4624);
#3806=AXIS2_PLACEMENT_3D('',#5770,#4625,#4626);
#3807=AXIS2_PLACEMENT_3D('',#5796,#4627,#4628);
#3808=AXIS2_PLACEMENT_3D('',#5820,#4629,#4630);
#3809=AXIS2_PLACEMENT_3D('',#5821,#4631,#4632);
#3810=AXIS2_PLACEMENT_3D('',#5823,#4633,#4634);
#3811=AXIS2_PLACEMENT_3D('',#5848,#4635,#4636);
#3812=AXIS2_PLACEMENT_3D('',#5873,#4637,#4638);
#3813=AXIS2_PLACEMENT_3D('',#5889,#4640,#4641);
#3814=AXIS2_PLACEMENT_3D('',#5904,#4642,#4643);
#3815=AXIS2_PLACEMENT_3D('',#5929,#4644,#4645);
#3816=AXIS2_PLACEMENT_3D('',#5954,#4646,#4647);
#3817=AXIS2_PLACEMENT_3D('',#5979,#4648,#4649);
#3818=AXIS2_PLACEMENT_3D('',#6003,#4650,#4651);
#3819=AXIS2_PLACEMENT_3D('',#6004,#4652,#4653);
#3820=AXIS2_PLACEMENT_3D('',#6006,#4654,#4655);
#3821=AXIS2_PLACEMENT_3D('',#6007,#4656,#4657);
#3822=AXIS2_PLACEMENT_3D('',#6008,#4658,#4659);
#3823=AXIS2_PLACEMENT_3D('',#6032,#4660,#4661);
#3824=AXIS2_PLACEMENT_3D('',#6033,#4662,#4663);
#3825=AXIS2_PLACEMENT_3D('',#6035,#4664,#4665);
#3826=AXIS2_PLACEMENT_3D('',#6036,#4666,#4667);
#3827=AXIS2_PLACEMENT_3D('',#6037,#4668,#4669);
#3828=AXIS2_PLACEMENT_3D('',#6061,#4670,#4671);
#3829=AXIS2_PLACEMENT_3D('',#6062,#4672,#4673);
#3830=AXIS2_PLACEMENT_3D('',#6064,#4674,#4675);
#3831=AXIS2_PLACEMENT_3D('',#6065,#4676,#4677);
#3832=AXIS2_PLACEMENT_3D('',#6066,#4678,#4679);
#3833=AXIS2_PLACEMENT_3D('',#6081,#4680,#4681);
#3834=AXIS2_PLACEMENT_3D('',#6094,#4682,#4683);
#3835=AXIS2_PLACEMENT_3D('',#6096,#4684,#4685);
#3836=AXIS2_PLACEMENT_3D('',#6097,#4686,#4687);
#3837=AXIS2_PLACEMENT_3D('',#6098,#4688,#4689);
#3838=AXIS2_PLACEMENT_3D('',#6122,#4690,#4691);
#3839=AXIS2_PLACEMENT_3D('',#6123,#4692,#4693);
#3840=AXIS2_PLACEMENT_3D('',#6125,#4694,#4695);
#3841=AXIS2_PLACEMENT_3D('',#6126,#4696,#4697);
#3842=AXIS2_PLACEMENT_3D('',#6127,#4698,#4699);
#3843=AXIS2_PLACEMENT_3D('',#6151,#4700,#4701);
#3844=AXIS2_PLACEMENT_3D('',#6152,#4702,#4703);
#3845=AXIS2_PLACEMENT_3D('',#6154,#4704,#4705);
#3846=AXIS2_PLACEMENT_3D('',#6155,#4706,#4707);
#3847=AXIS2_PLACEMENT_3D('',#6156,#4708,#4709);
#3848=AXIS2_PLACEMENT_3D('',#6180,#4710,#4711);
#3849=AXIS2_PLACEMENT_3D('',#6181,#4712,#4713);
#3850=AXIS2_PLACEMENT_3D('',#6183,#4714,#4715);
#3851=AXIS2_PLACEMENT_3D('',#6186,#4717,#4718);
#3852=AXIS2_PLACEMENT_3D('',#6210,#4719,#4720);
#3853=AXIS2_PLACEMENT_3D('',#6211,#4721,#4722);
#3854=AXIS2_PLACEMENT_3D('',#6212,#4723,#4724);
#3855=AXIS2_PLACEMENT_3D('',#6213,#4725,#4726);
#3856=AXIS2_PLACEMENT_3D('',#6214,#4727,#4728);
#3857=AXIS2_PLACEMENT_3D('',#6215,#4729,#4730);
#3858=AXIS2_PLACEMENT_3D('',#6216,#4731,#4732);
#3859=AXIS2_PLACEMENT_3D('',#6217,#4733,#4734);
#3860=AXIS2_PLACEMENT_3D('',#6218,#4735,#4736);
#3861=AXIS2_PLACEMENT_3D('',#6220,#4737,#4738);
#3862=AXIS2_PLACEMENT_3D('',#6222,#4739,#4740);
#3863=AXIS2_PLACEMENT_3D('',#6223,#4741,#4742);
#3864=AXIS2_PLACEMENT_3D('',#6225,#4743,#4744);
#3865=AXIS2_PLACEMENT_3D('',#6227,#4746,#4747);
#3866=AXIS2_PLACEMENT_3D('',#6229,#4748,#4749);
#3867=AXIS2_PLACEMENT_3D('',#6230,#4750,#4751);
#3868=AXIS2_PLACEMENT_3D('',#6232,#4753,#4754);
#3869=AXIS2_PLACEMENT_3D('',#6234,#4755,#4756);
#3870=AXIS2_PLACEMENT_3D('',#6236,#4757,#4758);
#3871=AXIS2_PLACEMENT_3D('',#6237,#4759,#4760);
#3872=AXIS2_PLACEMENT_3D('',#6239,#4761,#4762);
#3873=AXIS2_PLACEMENT_3D('',#6241,#4764,#4765);
#3874=AXIS2_PLACEMENT_3D('',#6243,#4766,#4767);
#3875=AXIS2_PLACEMENT_3D('',#6244,#4768,#4769);
#3876=AXIS2_PLACEMENT_3D('',#6246,#4771,#4772);
#3877=AXIS2_PLACEMENT_3D('',#6247,#4773,#4774);
#3878=AXIS2_PLACEMENT_3D('',#6248,#4775,#4776);
#3879=AXIS2_PLACEMENT_3D('',#6249,#4777,#4778);
#3880=AXIS2_PLACEMENT_3D('',#6250,#4779,#4780);
#3881=AXIS2_PLACEMENT_3D('',#6251,#4781,#4782);
#3882=AXIS2_PLACEMENT_3D('',#6252,#4783,#4784);
#3883=AXIS2_PLACEMENT_3D('',#6254,#4785,#4786);
#3884=AXIS2_PLACEMENT_3D('',#6257,#4788,#4789);
#3885=AXIS2_PLACEMENT_3D('',#6258,#4790,#4791);
#3886=AXIS2_PLACEMENT_3D('',#6260,#4792,#4793);
#3887=AXIS2_PLACEMENT_3D('',#6261,#4794,#4795);
#3888=AXIS2_PLACEMENT_3D('',#6263,#4796,#4797);
#3889=AXIS2_PLACEMENT_3D('',#6266,#4799,#4800);
#3890=AXIS2_PLACEMENT_3D('',#6267,#4801,#4802);
#3891=AXIS2_PLACEMENT_3D('',#6269,#4803,#4804);
#3892=AXIS2_PLACEMENT_3D('',#6270,#4805,#4806);
#3893=AXIS2_PLACEMENT_3D('',#6272,#4807,#4808);
#3894=AXIS2_PLACEMENT_3D('',#6275,#4810,#4811);
#3895=AXIS2_PLACEMENT_3D('',#6276,#4812,#4813);
#3896=AXIS2_PLACEMENT_3D('',#6278,#4814,#4815);
#3897=AXIS2_PLACEMENT_3D('',#6279,#4816,#4817);
#3898=AXIS2_PLACEMENT_3D('',#6281,#4818,#4819);
#3899=AXIS2_PLACEMENT_3D('',#6284,#4821,#4822);
#3900=AXIS2_PLACEMENT_3D('',#6285,#4823,#4824);
#3901=AXIS2_PLACEMENT_3D('',#6287,#4825,#4826);
#3902=AXIS2_PLACEMENT_3D('',#6288,#4827,#4828);
#3903=AXIS2_PLACEMENT_3D('',#6290,#4829,#4830);
#3904=AXIS2_PLACEMENT_3D('',#6292,#4832,#4833);
#3905=AXIS2_PLACEMENT_3D('',#6294,#4834,#4835);
#3906=AXIS2_PLACEMENT_3D('',#6296,#4837,#4838);
#3907=AXIS2_PLACEMENT_3D('',#6298,#4839,#4840);
#3908=AXIS2_PLACEMENT_3D('',#6300,#4842,#4843);
#3909=AXIS2_PLACEMENT_3D('',#6302,#4844,#4845);
#3910=AXIS2_PLACEMENT_3D('',#6304,#4847,#4848);
#3911=AXIS2_PLACEMENT_3D('',#6306,#4849,#4850);
#3912=AXIS2_PLACEMENT_3D('',#6309,#4852,#4853);
#3913=AXIS2_PLACEMENT_3D('',#6310,#4854,#4855);
#3914=AXIS2_PLACEMENT_3D('',#6312,#4856,#4857);
#3915=AXIS2_PLACEMENT_3D('',#6313,#4858,#4859);
#3916=AXIS2_PLACEMENT_3D('',#6315,#4860,#4861);
#3917=AXIS2_PLACEMENT_3D('',#6317,#4863,#4864);
#3918=AXIS2_PLACEMENT_3D('',#6319,#4865,#4866);
#3919=AXIS2_PLACEMENT_3D('',#6322,#4868,#4869);
#3920=AXIS2_PLACEMENT_3D('',#6323,#4870,#4871);
#3921=AXIS2_PLACEMENT_3D('',#6324,#4872,#4873);
#3922=AXIS2_PLACEMENT_3D('',#6325,#4874,#4875);
#3923=AXIS2_PLACEMENT_3D('',#6326,#4876,#4877);
#3924=AXIS2_PLACEMENT_3D('',#6335,#4882,#4883);
#3925=AXIS2_PLACEMENT_3D('',#6341,#4887,#4888);
#3926=AXIS2_PLACEMENT_3D('',#6347,#4892,#4893);
#3927=AXIS2_PLACEMENT_3D('',#6353,#4897,#4898);
#3928=AXIS2_PLACEMENT_3D('',#6359,#4902,#4903);
#3929=AXIS2_PLACEMENT_3D('',#6362,#4906,#4907);
#3930=AXIS2_PLACEMENT_3D('',#6363,#4908,#4909);
#3931=AXIS2_PLACEMENT_3D('',#6364,#4910,#4911);
#3932=AXIS2_PLACEMENT_3D('',#6366,#4912,#4913);
#3933=AXIS2_PLACEMENT_3D('',#6367,#4914,#4915);
#3934=AXIS2_PLACEMENT_3D('',#6369,#4916,#4917);
#3935=AXIS2_PLACEMENT_3D('',#6370,#4918,#4919);
#3936=AXIS2_PLACEMENT_3D('',#6372,#4920,#4921);
#3937=AXIS2_PLACEMENT_3D('',#6374,#4923,#4924);
#3938=AXIS2_PLACEMENT_3D('',#6376,#4925,#4926);
#3939=AXIS2_PLACEMENT_3D('',#6378,#4928,#4929);
#3940=AXIS2_PLACEMENT_3D('',#6380,#4930,#4931);
#3941=AXIS2_PLACEMENT_3D('',#6382,#4933,#4934);
#3942=AXIS2_PLACEMENT_3D('',#6384,#4935,#4936);
#3943=AXIS2_PLACEMENT_3D('',#6385,#4937,#4938);
#3944=AXIS2_PLACEMENT_3D('',#6387,#4939,#4940);
#3945=AXIS2_PLACEMENT_3D('',#6389,#4942,#4943);
#3946=AXIS2_PLACEMENT_3D('',#6391,#4945,#4946);
#3947=AXIS2_PLACEMENT_3D('',#6392,#4947,#4948);
#3948=AXIS2_PLACEMENT_3D('',#6393,#4949,#4950);
#3949=AXIS2_PLACEMENT_3D('',#6394,#4951,#4952);
#3950=AXIS2_PLACEMENT_3D('',#6395,#4953,#4954);
#3951=AXIS2_PLACEMENT_3D('',#6396,#4955,#4956);
#3952=AXIS2_PLACEMENT_3D('',#6397,#4957,#4958);
#3953=AXIS2_PLACEMENT_3D('',#6398,#4959,#4960);
#3954=AXIS2_PLACEMENT_3D('',#6399,#4961,#4962);
#3955=AXIS2_PLACEMENT_3D('',#6400,#4963,#4964);
#3956=AXIS2_PLACEMENT_3D('',#6401,#4965,#4966);
#3957=AXIS2_PLACEMENT_3D('',#6402,#4967,#4968);
#3958=AXIS2_PLACEMENT_3D('',#6403,#4969,#4970);
#3959=AXIS2_PLACEMENT_3D('',#6404,#4971,#4972);
#3960=AXIS2_PLACEMENT_3D('',#6405,#4973,#4974);
#3961=AXIS2_PLACEMENT_3D('',#6406,#4975,#4976);
#3962=AXIS2_PLACEMENT_3D('',#6407,#4977,#4978);
#3963=AXIS2_PLACEMENT_3D('',#6408,#4979,#4980);
#3964=AXIS2_PLACEMENT_3D('',#6409,#4981,#4982);
#3965=AXIS2_PLACEMENT_3D('',#6410,#4983,#4984);
#3966=AXIS2_PLACEMENT_3D('',#6411,#4985,#4986);
#3967=AXIS2_PLACEMENT_3D('',#6412,#4987,#4988);
#3968=AXIS2_PLACEMENT_3D('',#6413,#4989,#4990);
#3969=AXIS2_PLACEMENT_3D('',#6414,#4991,#4992);
#3970=AXIS2_PLACEMENT_3D('',#6415,#4993,#4994);
#3971=AXIS2_PLACEMENT_3D('',#6416,#4995,#4996);
#3972=AXIS2_PLACEMENT_3D('',#6421,#4998,#4999);
#3973=AXIS2_PLACEMENT_3D('',#6424,#5001,#5002);
#3974=AXIS2_PLACEMENT_3D('',#6425,#5003,#5004);
#3975=AXIS2_PLACEMENT_3D('',#6431,#5008,#5009);
#3976=AXIS2_PLACEMENT_3D('',#6434,#5011,#5012);
#3977=AXIS2_PLACEMENT_3D('',#6436,#5013,#5014);
#3978=AXIS2_PLACEMENT_3D('',#6438,#5015,#5016);
#3979=AXIS2_PLACEMENT_3D('',#6439,#5017,#5018);
#3980=AXIS2_PLACEMENT_3D('',#6441,#5019,#5020);
#3981=AXIS2_PLACEMENT_3D('',#6443,#5021,#5022);
#3982=AXIS2_PLACEMENT_3D('',#6444,#5023,#5024);
#3983=AXIS2_PLACEMENT_3D('',#6446,#5026,#5027);
#3984=AXIS2_PLACEMENT_3D('',#6449,#5029,#5030);
#3985=AXIS2_PLACEMENT_3D('',#6450,#5031,#5032);
#3986=AXIS2_PLACEMENT_3D('',#6451,#5033,#5034);
#3987=AXIS2_PLACEMENT_3D('',#6455,#5037,#5038);
#3988=AXIS2_PLACEMENT_3D('',#6456,#5039,#5040);
#3989=AXIS2_PLACEMENT_3D('',#6457,#5041,#5042);
#3990=AXIS2_PLACEMENT_3D('',#6459,#5043,#5044);
#3991=AXIS2_PLACEMENT_3D('',#6461,#5045,#5046);
#3992=AXIS2_PLACEMENT_3D('',#6462,#5047,#5048);
#3993=AXIS2_PLACEMENT_3D('',#6464,#5050,#5051);
#3994=AXIS2_PLACEMENT_3D('',#6467,#5053,#5054);
#3995=AXIS2_PLACEMENT_3D('',#6468,#5055,#5056);
#3996=AXIS2_PLACEMENT_3D('',#6469,#5057,#5058);
#3997=AXIS2_PLACEMENT_3D('',#6470,#5059,#5060);
#3998=AXIS2_PLACEMENT_3D('',#6471,#5061,#5062);
#3999=AXIS2_PLACEMENT_3D('',#6473,#5063,#5064);
#4000=AXIS2_PLACEMENT_3D('',#6476,#5066,#5067);
#4001=AXIS2_PLACEMENT_3D('',#6477,#5068,#5069);
#4002=AXIS2_PLACEMENT_3D('',#6479,#5070,#5071);
#4003=AXIS2_PLACEMENT_3D('',#6482,#5073,#5074);
#4004=AXIS2_PLACEMENT_3D('',#6483,#5075,#5076);
#4005=AXIS2_PLACEMENT_3D('',#6484,#5077,#5078);
#4006=AXIS2_PLACEMENT_3D('',#6485,#5079,#5080);
#4007=AXIS2_PLACEMENT_3D('',#6486,#5081,#5082);
#4008=AXIS2_PLACEMENT_3D('',#6490,#5084,#5085);
#4009=AXIS2_PLACEMENT_3D('',#6491,#5086,#5087);
#4010=AXIS2_PLACEMENT_3D('',#6508,#5088,#5089);
#4011=AXIS2_PLACEMENT_3D('',#6565,#5091,#5092);
#4012=AXIS2_PLACEMENT_3D('',#6567,#5094,#5095);
#4013=AXIS2_PLACEMENT_3D('',#6569,#5096,#5097);
#4014=AXIS2_PLACEMENT_3D('',#6572,#5099,#5100);
#4015=AXIS2_PLACEMENT_3D('',#6573,#5101,#5102);
#4016=AXIS2_PLACEMENT_3D('',#6575,#5103,#5104);
#4017=AXIS2_PLACEMENT_3D('',#6578,#5106,#5107);
#4018=AXIS2_PLACEMENT_3D('',#6579,#5108,#5109);
#4019=AXIS2_PLACEMENT_3D('',#6580,#5110,#5111);
#4020=AXIS2_PLACEMENT_3D('',#6581,#5112,#5113);
#4021=AXIS2_PLACEMENT_3D('',#6582,#5114,#5115);
#4022=AXIS2_PLACEMENT_3D('',#6584,#5116,#5117);
#4023=AXIS2_PLACEMENT_3D('',#6585,#5118,#5119);
#4024=AXIS2_PLACEMENT_3D('',#6594,#5124,#5125);
#4025=AXIS2_PLACEMENT_3D('',#6600,#5129,#5130);
#4026=AXIS2_PLACEMENT_3D('',#6606,#5134,#5135);
#4027=AXIS2_PLACEMENT_3D('',#6612,#5139,#5140);
#4028=AXIS2_PLACEMENT_3D('',#6618,#5144,#5145);
#4029=AXIS2_PLACEMENT_3D('',#6621,#5148,#5149);
#4030=AXIS2_PLACEMENT_3D('',#6622,#5150,#5151);
#4031=AXIS2_PLACEMENT_3D('',#6624,#5152,#5153);
#4032=AXIS2_PLACEMENT_3D('',#6625,#5154,#5155);
#4033=AXIS2_PLACEMENT_3D('',#6627,#5156,#5157);
#4034=AXIS2_PLACEMENT_3D('',#6629,#5159,#5160);
#4035=AXIS2_PLACEMENT_3D('',#6631,#5162,#5163);
#4036=AXIS2_PLACEMENT_3D('',#6632,#5164,#5165);
#4037=AXIS2_PLACEMENT_3D('',#6633,#5166,#5167);
#4038=AXIS2_PLACEMENT_3D('',#6634,#5168,#5169);
#4039=AXIS2_PLACEMENT_3D('',#6635,#5170,#5171);
#4040=AXIS2_PLACEMENT_3D('',#6636,#5172,#5173);
#4041=AXIS2_PLACEMENT_3D('',#6637,#5174,#5175);
#4042=AXIS2_PLACEMENT_3D('',#6638,#5176,#5177);
#4043=AXIS2_PLACEMENT_3D('',#6639,#5178,#5179);
#4044=AXIS2_PLACEMENT_3D('',#6640,#5180,#5181);
#4045=AXIS2_PLACEMENT_3D('',#6641,#5182,#5183);
#4046=AXIS2_PLACEMENT_3D('',#6642,#5184,#5185);
#4047=AXIS2_PLACEMENT_3D('',#6643,#5186,#5187);
#4048=AXIS2_PLACEMENT_3D('',#6644,#5188,#5189);
#4049=AXIS2_PLACEMENT_3D('',#6645,#5190,#5191);
#4050=AXIS2_PLACEMENT_3D('',#6646,#5192,#5193);
#4051=AXIS2_PLACEMENT_3D('',#6647,#5194,#5195);
#4052=AXIS2_PLACEMENT_3D('',#6648,#5196,#5197);
#4053=AXIS2_PLACEMENT_3D('',#6649,#5198,#5199);
#4054=AXIS2_PLACEMENT_3D('',#6650,#5200,#5201);
#4055=AXIS2_PLACEMENT_3D('',#6651,#5202,#5203);
#4056=AXIS2_PLACEMENT_3D('',#6652,#5204,#5205);
#4057=AXIS2_PLACEMENT_3D('',#6653,#5206,#5207);
#4058=AXIS2_PLACEMENT_3D('',#6654,#5208,#5209);
#4059=AXIS2_PLACEMENT_3D('',#6655,#5210,#5211);
#4060=AXIS2_PLACEMENT_3D('',#6656,#5212,#5213);
#4061=AXIS2_PLACEMENT_3D('',#6657,#5214,#5215);
#4062=AXIS2_PLACEMENT_3D('',#6658,#5216,#5217);
#4063=AXIS2_PLACEMENT_3D('',#6659,#5218,#5219);
#4064=AXIS2_PLACEMENT_3D('',#6660,#5220,#5221);
#4065=AXIS2_PLACEMENT_3D('',#6661,#5222,#5223);
#4066=DIRECTION('axis',(0.,0.,1.));
#4067=DIRECTION('refdir',(1.,0.,0.));
#4068=DIRECTION('axis',(0.,0.,1.));
#4069=DIRECTION('refdir',(1.,0.,0.));
#4070=DIRECTION('axis',(0.,0.,1.));
#4071=DIRECTION('refdir',(1.,0.,0.));
#4072=DIRECTION('center_axis',(0.,0.,1.));
#4073=DIRECTION('ref_axis',(1.,0.,0.));
#4074=DIRECTION('center_axis',(0.,0.,1.));
#4075=DIRECTION('ref_axis',(1.,0.,0.));
#4076=DIRECTION('',(0.,0.,1.));
#4077=DIRECTION('center_axis',(0.,0.,-1.));
#4078=DIRECTION('ref_axis',(1.,0.,0.));
#4079=DIRECTION('center_axis',(0.,0.,1.));
#4080=DIRECTION('ref_axis',(1.,0.,0.));
#4081=DIRECTION('center_axis',(0.,0.,1.));
#4082=DIRECTION('ref_axis',(1.,0.,0.));
#4083=DIRECTION('',(0.,0.,1.));
#4084=DIRECTION('center_axis',(0.,0.,-1.));
#4085=DIRECTION('ref_axis',(1.,0.,0.));
#4086=DIRECTION('center_axis',(0.,0.,1.));
#4087=DIRECTION('ref_axis',(1.,0.,0.));
#4088=DIRECTION('center_axis',(0.,0.,1.));
#4089=DIRECTION('ref_axis',(1.,0.,0.));
#4090=DIRECTION('',(0.,0.,1.));
#4091=DIRECTION('center_axis',(0.,0.,-1.));
#4092=DIRECTION('ref_axis',(1.,0.,0.));
#4093=DIRECTION('center_axis',(0.,0.,1.));
#4094=DIRECTION('ref_axis',(1.,0.,0.));
#4095=DIRECTION('center_axis',(0.,0.,1.));
#4096=DIRECTION('ref_axis',(1.,0.,0.));
#4097=DIRECTION('',(0.,0.,1.));
#4098=DIRECTION('center_axis',(0.,0.,-1.));
#4099=DIRECTION('ref_axis',(1.,0.,0.));
#4100=DIRECTION('center_axis',(0.,0.,1.));
#4101=DIRECTION('ref_axis',(1.,0.,0.));
#4102=DIRECTION('center_axis',(0.,0.,1.));
#4103=DIRECTION('ref_axis',(1.,0.,0.));
#4104=DIRECTION('',(0.,0.,1.));
#4105=DIRECTION('center_axis',(0.,0.,-1.));
#4106=DIRECTION('ref_axis',(1.,0.,0.));
#4107=DIRECTION('center_axis',(0.,0.,1.));
#4108=DIRECTION('ref_axis',(1.,0.,0.));
#4109=DIRECTION('center_axis',(0.,0.,1.));
#4110=DIRECTION('ref_axis',(1.,0.,0.));
#4111=DIRECTION('',(0.,0.,1.));
#4112=DIRECTION('center_axis',(0.,0.,-1.));
#4113=DIRECTION('ref_axis',(1.,0.,0.));
#4114=DIRECTION('center_axis',(0.,0.,1.));
#4115=DIRECTION('ref_axis',(1.,0.,0.));
#4116=DIRECTION('center_axis',(0.,0.,1.));
#4117=DIRECTION('ref_axis',(1.,0.,0.));
#4118=DIRECTION('',(0.,0.,1.));
#4119=DIRECTION('center_axis',(0.,0.,-1.));
#4120=DIRECTION('ref_axis',(1.,0.,0.));
#4121=DIRECTION('center_axis',(0.,0.,1.));
#4122=DIRECTION('ref_axis',(1.,0.,0.));
#4123=DIRECTION('center_axis',(0.,0.,1.));
#4124=DIRECTION('ref_axis',(1.,0.,0.));
#4125=DIRECTION('',(0.,0.,1.));
#4126=DIRECTION('center_axis',(0.,0.,-1.));
#4127=DIRECTION('ref_axis',(1.,0.,0.));
#4128=DIRECTION('center_axis',(0.,1.,0.));
#4129=DIRECTION('ref_axis',(-1.,0.,0.));
#4130=DIRECTION('',(-1.,0.,0.));
#4131=DIRECTION('',(0.,0.,1.));
#4132=DIRECTION('',(-1.,0.,0.));
#4133=DIRECTION('',(0.,0.,1.));
#4134=DIRECTION('center_axis',(1.,0.,0.));
#4135=DIRECTION('ref_axis',(0.,1.,0.));
#4136=DIRECTION('',(0.,1.,0.));
#4137=DIRECTION('',(0.,1.,0.));
#4138=DIRECTION('',(0.,0.,1.));
#4139=DIRECTION('center_axis',(0.,-1.,0.));
#4140=DIRECTION('ref_axis',(1.,0.,0.));
#4141=DIRECTION('',(1.,0.,0.));
#4142=DIRECTION('',(1.,0.,0.));
#4143=DIRECTION('',(0.,0.,1.));
#4144=DIRECTION('center_axis',(-1.,0.,0.));
#4145=DIRECTION('ref_axis',(0.,-1.,0.));
#4146=DIRECTION('',(0.,-1.,0.));
#4147=DIRECTION('',(0.,-1.,0.));
#4148=DIRECTION('center_axis',(0.,0.,1.));
#4149=DIRECTION('ref_axis',(1.,0.,0.));
#4150=DIRECTION('center_axis',(0.,0.,1.));
#4151=DIRECTION('ref_axis',(1.,0.,0.));
#4152=DIRECTION('axis',(0.,0.,1.));
#4153=DIRECTION('refdir',(1.,0.,0.));
#4154=DIRECTION('center_axis',(1.,0.,0.));
#4155=DIRECTION('ref_axis',(0.,0.,-1.));
#4156=DIRECTION('',(1.,0.,0.));
#4157=DIRECTION('center_axis',(0.,0.,1.));
#4158=DIRECTION('ref_axis',(1.,0.,0.));
#4159=DIRECTION('center_axis',(0.,0.,1.));
#4160=DIRECTION('ref_axis',(1.,0.,0.));
#4161=DIRECTION('',(0.,0.,1.));
#4162=DIRECTION('center_axis',(0.,0.,-1.));
#4163=DIRECTION('ref_axis',(1.,0.,0.));
#4164=DIRECTION('center_axis',(0.,0.,1.));
#4165=DIRECTION('ref_axis',(1.,0.,0.));
#4166=DIRECTION('center_axis',(0.,0.,1.));
#4167=DIRECTION('ref_axis',(1.,0.,0.));
#4168=DIRECTION('center_axis',(0.,0.,1.));
#4169=DIRECTION('ref_axis',(1.,0.,0.));
#4170=DIRECTION('',(0.,0.,1.));
#4171=DIRECTION('center_axis',(0.,0.,-1.));
#4172=DIRECTION('ref_axis',(1.,0.,0.));
#4173=DIRECTION('center_axis',(0.,0.,1.));
#4174=DIRECTION('ref_axis',(1.,0.,0.));
#4175=DIRECTION('center_axis',(0.,0.,1.));
#4176=DIRECTION('ref_axis',(1.,0.,0.));
#4177=DIRECTION('center_axis',(0.,0.,1.));
#4178=DIRECTION('ref_axis',(1.,0.,0.));
#4179=DIRECTION('',(0.,0.,1.));
#4180=DIRECTION('center_axis',(0.,0.,-1.));
#4181=DIRECTION('ref_axis',(1.,0.,0.));
#4182=DIRECTION('center_axis',(0.,0.,1.));
#4183=DIRECTION('ref_axis',(1.,0.,0.));
#4184=DIRECTION('center_axis',(0.,0.,1.));
#4185=DIRECTION('ref_axis',(1.,0.,0.));
#4186=DIRECTION('center_axis',(0.,0.,1.));
#4187=DIRECTION('ref_axis',(1.,0.,0.));
#4188=DIRECTION('',(0.,0.,1.));
#4189=DIRECTION('center_axis',(0.,0.,-1.));
#4190=DIRECTION('ref_axis',(1.,0.,0.));
#4191=DIRECTION('center_axis',(0.,0.,1.));
#4192=DIRECTION('ref_axis',(1.,0.,0.));
#4193=DIRECTION('center_axis',(0.,0.,1.));
#4194=DIRECTION('ref_axis',(1.,0.,0.));
#4195=DIRECTION('center_axis',(0.,0.,1.));
#4196=DIRECTION('ref_axis',(1.,0.,0.));
#4197=DIRECTION('center_axis',(0.,0.,1.));
#4198=DIRECTION('ref_axis',(1.,0.,0.));
#4199=DIRECTION('center_axis',(0.,0.,1.));
#4200=DIRECTION('ref_axis',(1.,0.,0.));
#4201=DIRECTION('',(0.,0.,1.));
#4202=DIRECTION('center_axis',(0.,0.,1.));
#4203=DIRECTION('ref_axis',(1.,0.,0.));
#4204=DIRECTION('',(0.,0.,-1.));
#4205=DIRECTION('center_axis',(0.,0.,1.));
#4206=DIRECTION('ref_axis',(1.,0.,0.));
#4207=DIRECTION('',(0.,0.,-1.));
#4208=DIRECTION('center_axis',(0.,0.,1.));
#4209=DIRECTION('ref_axis',(1.,0.,0.));
#4210=DIRECTION('',(0.,0.,1.));
#4211=DIRECTION('center_axis',(0.,0.,1.));
#4212=DIRECTION('ref_axis',(1.,0.,0.));
#4213=DIRECTION('center_axis',(0.,0.,1.));
#4214=DIRECTION('ref_axis',(1.,0.,0.));
#4215=DIRECTION('center_axis',(0.,0.,1.));
#4216=DIRECTION('ref_axis',(1.,0.,0.));
#4217=DIRECTION('center_axis',(0.,0.,1.));
#4218=DIRECTION('ref_axis',(-0.707106781186548,-0.707106781186547,0.));
#4219=DIRECTION('',(0.,0.,-1.));
#4220=DIRECTION('center_axis',(0.,0.,1.));
#4221=DIRECTION('ref_axis',(1.,0.,0.));
#4222=DIRECTION('',(0.,0.,1.));
#4223=DIRECTION('center_axis',(0.,0.,1.));
#4224=DIRECTION('ref_axis',(1.,0.,0.));
#4225=DIRECTION('center_axis',(0.,0.,1.));
#4226=DIRECTION('ref_axis',(1.,0.,0.));
#4227=DIRECTION('center_axis',(0.,0.,1.));
#4228=DIRECTION('ref_axis',(1.,0.,0.));
#4229=DIRECTION('center_axis',(0.,0.,1.));
#4230=DIRECTION('ref_axis',(-0.707106781186547,0.707106781186548,0.));
#4231=DIRECTION('',(0.,0.,-1.));
#4232=DIRECTION('center_axis',(0.,0.,1.));
#4233=DIRECTION('ref_axis',(1.,0.,0.));
#4234=DIRECTION('',(0.,0.,1.));
#4235=DIRECTION('center_axis',(0.,0.,1.));
#4236=DIRECTION('ref_axis',(1.,0.,0.));
#4237=DIRECTION('center_axis',(0.,0.,1.));
#4238=DIRECTION('ref_axis',(1.,0.,0.));
#4239=DIRECTION('center_axis',(0.,0.,1.));
#4240=DIRECTION('ref_axis',(1.,0.,0.));
#4241=DIRECTION('center_axis',(0.,0.,1.));
#4242=DIRECTION('ref_axis',(1.,0.,0.));
#4243=DIRECTION('center_axis',(0.,0.,1.));
#4244=DIRECTION('ref_axis',(1.,0.,0.));
#4245=DIRECTION('',(0.,0.,-1.));
#4246=DIRECTION('center_axis',(0.,0.,1.));
#4247=DIRECTION('ref_axis',(1.,0.,0.));
#4248=DIRECTION('center_axis',(0.,0.,1.));
#4249=DIRECTION('ref_axis',(1.,0.,0.));
#4250=DIRECTION('center_axis',(0.,0.,1.));
#4251=DIRECTION('ref_axis',(1.,0.,0.));
#4252=DIRECTION('center_axis',(0.,0.,1.));
#4253=DIRECTION('ref_axis',(1.,0.,0.));
#4254=DIRECTION('center_axis',(0.,0.,1.));
#4255=DIRECTION('ref_axis',(1.,0.,0.));
#4256=DIRECTION('center_axis',(0.,0.,1.));
#4257=DIRECTION('ref_axis',(1.,0.,0.));
#4258=DIRECTION('center_axis',(0.,0.,1.));
#4259=DIRECTION('ref_axis',(1.,0.,0.));
#4260=DIRECTION('center_axis',(0.,0.,-1.));
#4261=DIRECTION('ref_axis',(1.,0.,0.));
#4262=DIRECTION('center_axis',(0.,0.,-1.));
#4263=DIRECTION('ref_axis',(1.,0.,0.));
#4264=DIRECTION('center_axis',(0.,0.,-1.));
#4265=DIRECTION('ref_axis',(1.,0.,0.));
#4266=DIRECTION('center_axis',(0.,0.,-1.));
#4267=DIRECTION('ref_axis',(1.,0.,0.));
#4268=DIRECTION('center_axis',(0.,0.,1.));
#4269=DIRECTION('ref_axis',(1.,0.,0.));
#4270=DIRECTION('center_axis',(0.,0.,1.));
#4271=DIRECTION('ref_axis',(1.,0.,0.));
#4272=DIRECTION('',(0.,0.,1.));
#4273=DIRECTION('center_axis',(0.,0.,1.));
#4274=DIRECTION('ref_axis',(1.,0.,0.));
#4275=DIRECTION('center_axis',(0.,0.,1.));
#4276=DIRECTION('ref_axis',(1.,0.,0.));
#4277=DIRECTION('',(0.,0.,1.));
#4278=DIRECTION('center_axis',(0.,0.,1.));
#4279=DIRECTION('ref_axis',(1.,0.,0.));
#4280=DIRECTION('center_axis',(0.,0.,1.));
#4281=DIRECTION('ref_axis',(1.,0.,0.));
#4282=DIRECTION('',(0.,0.,1.));
#4283=DIRECTION('center_axis',(0.,0.,1.));
#4284=DIRECTION('ref_axis',(1.,0.,0.));
#4285=DIRECTION('center_axis',(0.,0.,1.));
#4286=DIRECTION('ref_axis',(1.,0.,0.));
#4287=DIRECTION('',(0.,0.,1.));
#4288=DIRECTION('center_axis',(0.,0.,1.));
#4289=DIRECTION('ref_axis',(1.,0.,0.));
#4290=DIRECTION('center_axis',(0.,0.,1.));
#4291=DIRECTION('ref_axis',(1.,0.,0.));
#4292=DIRECTION('',(0.,0.,1.));
#4293=DIRECTION('center_axis',(0.,0.,-1.));
#4294=DIRECTION('ref_axis',(1.,0.,0.));
#4295=DIRECTION('center_axis',(0.,0.,1.));
#4296=DIRECTION('ref_axis',(1.,0.,0.));
#4297=DIRECTION('center_axis',(0.,0.,1.));
#4298=DIRECTION('ref_axis',(1.,0.,0.));
#4299=DIRECTION('center_axis',(0.,0.,1.));
#4300=DIRECTION('ref_axis',(1.,0.,0.));
#4301=DIRECTION('',(0.,0.,-1.));
#4302=DIRECTION('center_axis',(0.,0.,1.));
#4303=DIRECTION('ref_axis',(1.,0.,0.));
#4304=DIRECTION('center_axis',(0.,0.,1.));
#4305=DIRECTION('ref_axis',(1.,0.,0.));
#4306=DIRECTION('',(0.,0.,-1.));
#4307=DIRECTION('center_axis',(0.,0.,-1.));
#4308=DIRECTION('ref_axis',(1.,0.,0.));
#4309=DIRECTION('center_axis',(0.,0.,1.));
#4310=DIRECTION('ref_axis',(1.,0.,0.));
#4311=DIRECTION('center_axis',(0.,0.,1.));
#4312=DIRECTION('ref_axis',(1.,0.,0.));
#4313=DIRECTION('axis',(0.,0.,1.));
#4314=DIRECTION('refdir',(1.,0.,0.));
#4315=DIRECTION('center_axis',(0.866025403784439,0.,-0.5));
#4316=DIRECTION('ref_axis',(0.5,0.,0.866025403784439));
#4317=DIRECTION('',(-0.5,0.,-0.866025403784439));
#4318=DIRECTION('',(0.,-1.,0.));
#4319=DIRECTION('',(0.5,0.,0.866025403784439));
#4320=DIRECTION('',(0.,-1.,0.));
#4321=DIRECTION('center_axis',(1.20185167898973E-16,0.,-1.));
#4322=DIRECTION('ref_axis',(1.,0.,1.20185167898973E-16));
#4323=DIRECTION('',(-1.,0.,-1.20185167898973E-16));
#4324=DIRECTION('',(0.,-1.,0.));
#4325=DIRECTION('',(1.,0.,1.20185167898973E-16));
#4326=DIRECTION('center_axis',(-0.866025403784439,0.,-0.5));
#4327=DIRECTION('ref_axis',(0.5,0.,-0.866025403784439));
#4328=DIRECTION('',(-0.5,0.,0.866025403784439));
#4329=DIRECTION('',(0.,-1.,0.));
#4330=DIRECTION('',(0.5,0.,-0.866025403784439));
#4331=DIRECTION('center_axis',(-0.866025403784439,0.,0.5));
#4332=DIRECTION('ref_axis',(-0.5,0.,-0.866025403784439));
#4333=DIRECTION('',(0.5,0.,0.866025403784439));
#4334=DIRECTION('',(0.,-1.,0.));
#4335=DIRECTION('',(-0.5,0.,-0.866025403784439));
#4336=DIRECTION('center_axis',(-2.40370335797945E-16,0.,1.));
#4337=DIRECTION('ref_axis',(-1.,0.,-2.40370335797945E-16));
#4338=DIRECTION('',(1.,0.,2.40370335797945E-16));
#4339=DIRECTION('',(0.,-1.,0.));
#4340=DIRECTION('',(-1.,0.,-2.40370335797945E-16));
#4341=DIRECTION('center_axis',(0.866025403784439,0.,0.5));
#4342=DIRECTION('ref_axis',(-0.5,0.,0.866025403784439));
#4343=DIRECTION('',(0.5,0.,-0.866025403784439));
#4344=DIRECTION('',(-0.5,0.,0.866025403784439));
#4345=DIRECTION('center_axis',(0.,1.,0.));
#4346=DIRECTION('ref_axis',(1.,0.,0.));
#4347=DIRECTION('center_axis',(0.,-1.,0.));
#4348=DIRECTION('ref_axis',(0.,0.,-1.));
#4349=DIRECTION('center_axis',(0.,1.,0.));
#4350=DIRECTION('ref_axis',(1.,0.,0.));
#4351=DIRECTION('center_axis',(0.,1.,0.));
#4352=DIRECTION('ref_axis',(1.,0.,0.));
#4353=DIRECTION('center_axis',(0.,1.,0.));
#4354=DIRECTION('ref_axis',(0.,0.,1.));
#4355=DIRECTION('center_axis',(0.,-1.,0.));
#4356=DIRECTION('ref_axis',(1.,0.,0.));
#4357=DIRECTION('center_axis',(0.,-1.,0.));
#4358=DIRECTION('ref_axis',(1.,0.,0.));
#4359=DIRECTION('center_axis',(0.,-1.,0.));
#4360=DIRECTION('ref_axis',(1.,0.,0.));
#4361=DIRECTION('',(0.707106781186548,0.707106781186547,8.65956056235493E-17));
#4362=DIRECTION('center_axis',(0.,-1.,0.));
#4363=DIRECTION('ref_axis',(1.,0.,0.));
#4364=DIRECTION('center_axis',(0.,-1.,0.));
#4365=DIRECTION('ref_axis',(1.,0.,0.));
#4366=DIRECTION('',(0.,1.,0.));
#4367=DIRECTION('center_axis',(0.,1.,0.));
#4368=DIRECTION('ref_axis',(1.,0.,0.));
#4369=DIRECTION('center_axis',(0.,-1.,0.));
#4370=DIRECTION('ref_axis',(1.,0.,0.));
#4371=DIRECTION('',(-0.707106781186547,0.707106781186548,-8.65956056235493E-17));
#4372=DIRECTION('center_axis',(0.,-1.,0.));
#4373=DIRECTION('ref_axis',(0.,0.,-1.));
#4374=DIRECTION('center_axis',(0.,-1.,0.));
#4375=DIRECTION('ref_axis',(1.,0.,0.));
#4376=DIRECTION('center_axis',(0.,1.,0.));
#4377=DIRECTION('ref_axis',(1.,0.,0.));
#4378=DIRECTION('center_axis',(0.,1.,0.));
#4379=DIRECTION('ref_axis',(1.,0.,0.));
#4380=DIRECTION('',(-0.447213595499958,0.894427190999916,-5.47678698264203E-17));
#4381=DIRECTION('center_axis',(0.,-1.,0.));
#4382=DIRECTION('ref_axis',(1.,0.,0.));
#4383=DIRECTION('',(0.,1.,0.));
#4384=DIRECTION('axis',(0.,0.,1.));
#4385=DIRECTION('refdir',(1.,0.,0.));
#4386=DIRECTION('axis',(0.,0.,1.));
#4387=DIRECTION('refdir',(1.,0.,0.));
#4388=DIRECTION('axis',(0.,0.,1.));
#4389=DIRECTION('refdir',(1.,0.,0.));
#4390=DIRECTION('center_axis',(0.,0.,1.));
#4391=DIRECTION('ref_axis',(1.,0.,0.));
#4392=DIRECTION('center_axis',(0.,0.,1.));
#4393=DIRECTION('ref_axis',(1.,0.,0.));
#4394=DIRECTION('',(0.,0.,1.));
#4395=DIRECTION('center_axis',(0.,0.,-1.));
#4396=DIRECTION('ref_axis',(1.,0.,0.));
#4397=DIRECTION('center_axis',(0.,0.,1.));
#4398=DIRECTION('ref_axis',(1.,0.,0.));
#4399=DIRECTION('center_axis',(0.,0.,1.));
#4400=DIRECTION('ref_axis',(1.,0.,0.));
#4401=DIRECTION('center_axis',(0.,0.,1.));
#4402=DIRECTION('ref_axis',(1.,0.,0.));
#4403=DIRECTION('',(0.,0.,1.));
#4404=DIRECTION('center_axis',(0.,0.,-1.));
#4405=DIRECTION('ref_axis',(1.,0.,0.));
#4406=DIRECTION('center_axis',(0.,0.,1.));
#4407=DIRECTION('ref_axis',(1.,0.,0.));
#4408=DIRECTION('center_axis',(0.,0.,1.));
#4409=DIRECTION('ref_axis',(1.,0.,0.));
#4410=DIRECTION('center_axis',(0.,0.,1.));
#4411=DIRECTION('ref_axis',(1.,0.,0.));
#4412=DIRECTION('',(0.,0.,1.));
#4413=DIRECTION('center_axis',(0.,0.,-1.));
#4414=DIRECTION('ref_axis',(1.,0.,0.));
#4415=DIRECTION('center_axis',(0.,0.,1.));
#4416=DIRECTION('ref_axis',(1.,0.,0.));
#4417=DIRECTION('center_axis',(0.,0.,1.));
#4418=DIRECTION('ref_axis',(1.,0.,0.));
#4419=DIRECTION('center_axis',(0.,0.,1.));
#4420=DIRECTION('ref_axis',(1.,0.,0.));
#4421=DIRECTION('',(0.,0.,1.));
#4422=DIRECTION('center_axis',(0.,0.,-1.));
#4423=DIRECTION('ref_axis',(1.,0.,0.));
#4424=DIRECTION('center_axis',(0.,0.,1.));
#4425=DIRECTION('ref_axis',(1.,0.,0.));
#4426=DIRECTION('center_axis',(0.,0.,1.));
#4427=DIRECTION('ref_axis',(1.,0.,0.));
#4428=DIRECTION('center_axis',(0.,0.,1.));
#4429=DIRECTION('ref_axis',(1.,0.,0.));
#4430=DIRECTION('',(0.,0.,1.));
#4431=DIRECTION('center_axis',(0.,0.,-1.));
#4432=DIRECTION('ref_axis',(1.,0.,0.));
#4433=DIRECTION('center_axis',(0.,0.,1.));
#4434=DIRECTION('ref_axis',(1.,0.,0.));
#4435=DIRECTION('center_axis',(0.,0.,1.));
#4436=DIRECTION('ref_axis',(1.,0.,0.));
#4437=DIRECTION('center_axis',(0.,0.,1.));
#4438=DIRECTION('ref_axis',(1.,0.,0.));
#4439=DIRECTION('center_axis',(0.,0.,1.));
#4440=DIRECTION('ref_axis',(1.,0.,0.));
#4441=DIRECTION('',(0.,0.,1.));
#4442=DIRECTION('center_axis',(0.,0.,1.));
#4443=DIRECTION('ref_axis',(1.,0.,0.));
#4444=DIRECTION('center_axis',(0.,0.,1.));
#4445=DIRECTION('ref_axis',(1.,0.,0.));
#4446=DIRECTION('',(0.,0.,-1.));
#4447=DIRECTION('center_axis',(0.,0.,1.));
#4448=DIRECTION('ref_axis',(1.,0.,0.));
#4449=DIRECTION('',(0.,0.,-1.));
#4450=DIRECTION('center_axis',(0.,0.,-1.));
#4451=DIRECTION('ref_axis',(1.,0.,0.));
#4452=DIRECTION('',(0.,0.,1.));
#4453=DIRECTION('center_axis',(0.,0.,1.));
#4454=DIRECTION('ref_axis',(1.,0.,0.));
#4455=DIRECTION('center_axis',(0.,0.,1.));
#4456=DIRECTION('ref_axis',(1.,0.,0.));
#4457=DIRECTION('center_axis',(0.,0.,1.));
#4458=DIRECTION('ref_axis',(1.,0.,0.));
#4459=DIRECTION('center_axis',(0.866025403784439,-0.5,0.));
#4460=DIRECTION('ref_axis',(0.5,0.866025403784439,0.));
#4461=DIRECTION('',(0.5,0.866025403784439,0.));
#4462=DIRECTION('',(0.,0.,1.));
#4463=DIRECTION('',(-0.5,-0.866025403784439,0.));
#4464=DIRECTION('center_axis',(0.,0.,1.));
#4465=DIRECTION('ref_axis',(1.,0.,0.));
#4466=DIRECTION('',(-0.5,-0.866025403784439,0.));
#4467=DIRECTION('center_axis',(0.,0.,1.));
#4468=DIRECTION('ref_axis',(1.,0.,0.));
#4469=DIRECTION('center_axis',(-0.866025403784439,0.5,0.));
#4470=DIRECTION('ref_axis',(-0.5,-0.866025403784439,0.));
#4471=DIRECTION('',(0.5,0.866025403784439,0.));
#4472=DIRECTION('',(0.,0.,-1.));
#4473=DIRECTION('center_axis',(0.,0.,1.));
#4474=DIRECTION('ref_axis',(-0.5,-0.866025403784438,0.));
#4475=DIRECTION('center_axis',(0.,0.,1.));
#4476=DIRECTION('ref_axis',(1.,0.,0.));
#4477=DIRECTION('center_axis',(0.,0.,1.));
#4478=DIRECTION('ref_axis',(1.,0.,0.));
#4479=DIRECTION('center_axis',(0.,0.,1.));
#4480=DIRECTION('ref_axis',(1.,0.,0.));
#4481=DIRECTION('center_axis',(0.,0.,1.));
#4482=DIRECTION('ref_axis',(1.,0.,0.));
#4483=DIRECTION('center_axis',(0.,0.,1.));
#4484=DIRECTION('ref_axis',(1.,0.,0.));
#4485=DIRECTION('center_axis',(0.,0.,-1.));
#4486=DIRECTION('ref_axis',(1.,0.,0.));
#4487=DIRECTION('center_axis',(0.,0.,1.));
#4488=DIRECTION('ref_axis',(1.,0.,0.));
#4489=DIRECTION('',(0.,0.,-1.));
#4490=DIRECTION('center_axis',(0.,0.,1.));
#4491=DIRECTION('ref_axis',(1.,0.,0.));
#4492=DIRECTION('',(0.,0.,-1.));
#4493=DIRECTION('center_axis',(0.,0.,1.));
#4494=DIRECTION('ref_axis',(1.,0.,0.));
#4495=DIRECTION('center_axis',(0.,0.,1.));
#4496=DIRECTION('ref_axis',(1.,0.,0.));
#4497=DIRECTION('axis',(0.,0.,1.));
#4498=DIRECTION('refdir',(1.,0.,0.));
#4499=DIRECTION('axis',(0.,0.,1.));
#4500=DIRECTION('refdir',(1.,0.,0.));
#4501=DIRECTION('center_axis',(0.,-1.,0.));
#4502=DIRECTION('ref_axis',(0.,0.,-1.));
#4503=DIRECTION('center_axis',(0.,-1.,0.));
#4504=DIRECTION('ref_axis',(1.,0.,0.));
#4505=DIRECTION('center_axis',(0.,-1.,0.));
#4506=DIRECTION('ref_axis',(1.,0.,0.));
#4507=DIRECTION('center_axis',(1.,0.,1.22464679914735E-16));
#4508=DIRECTION('ref_axis',(-1.22464679914735E-16,0.,1.));
#4509=DIRECTION('center_axis',(0.,1.,0.));
#4510=DIRECTION('ref_axis',(1.,0.,0.));
#4511=DIRECTION('center_axis',(0.,1.,0.));
#4512=DIRECTION('ref_axis',(1.,0.,0.));
#4513=DIRECTION('center_axis',(0.,-1.,0.));
#4514=DIRECTION('ref_axis',(1.,0.,0.));
#4515=DIRECTION('',(0.,1.,0.));
#4516=DIRECTION('center_axis',(0.,-1.,0.));
#4517=DIRECTION('ref_axis',(1.,0.,0.));
#4518=DIRECTION('center_axis',(0.,-1.,0.));
#4519=DIRECTION('ref_axis',(1.,0.,0.));
#4520=DIRECTION('center_axis',(0.,-1.,0.));
#4521=DIRECTION('ref_axis',(1.,0.,0.));
#4522=DIRECTION('',(0.,1.,0.));
#4523=DIRECTION('center_axis',(0.,-1.,0.));
#4524=DIRECTION('ref_axis',(1.,0.,0.));
#4525=DIRECTION('center_axis',(0.,1.,0.));
#4526=DIRECTION('ref_axis',(1.,0.,0.));
#4527=DIRECTION('',(-0.707106781186547,0.707106781186548,-8.65956056235493E-17));
#4528=DIRECTION('center_axis',(0.,-1.,0.));
#4529=DIRECTION('ref_axis',(1.,0.,0.));
#4530=DIRECTION('center_axis',(0.,1.,0.));
#4531=DIRECTION('ref_axis',(0.,0.,1.));
#4532=DIRECTION('center_axis',(0.,-1.,0.));
#4533=DIRECTION('ref_axis',(1.,0.,0.));
#4534=DIRECTION('center_axis',(0.,-1.,0.));
#4535=DIRECTION('ref_axis',(1.,0.,0.));
#4536=DIRECTION('',(0.,1.,0.));
#4537=DIRECTION('center_axis',(0.,-1.,0.));
#4538=DIRECTION('ref_axis',(0.,0.,-1.));
#4539=DIRECTION('center_axis',(0.,-1.,0.));
#4540=DIRECTION('ref_axis',(1.,0.,0.));
#4541=DIRECTION('center_axis',(0.,-1.,0.));
#4542=DIRECTION('ref_axis',(1.,0.,0.));
#4543=DIRECTION('',(0.707106781186547,0.707106781186548,8.65956056235493E-17));
#4544=DIRECTION('axis',(0.,0.,1.));
#4545=DIRECTION('refdir',(1.,0.,0.));
#4546=DIRECTION('center_axis',(0.,-1.,0.));
#4547=DIRECTION('ref_axis',(0.,0.,-1.));
#4548=DIRECTION('center_axis',(0.,-1.,0.));
#4549=DIRECTION('ref_axis',(1.,0.,0.));
#4550=DIRECTION('center_axis',(0.,-1.,0.));
#4551=DIRECTION('ref_axis',(1.,0.,0.));
#4552=DIRECTION('center_axis',(1.,0.,1.22464679914735E-16));
#4553=DIRECTION('ref_axis',(-1.22464679914735E-16,0.,1.));
#4554=DIRECTION('center_axis',(0.,1.,0.));
#4555=DIRECTION('ref_axis',(1.,0.,0.));
#4556=DIRECTION('center_axis',(0.,1.,0.));
#4557=DIRECTION('ref_axis',(1.,0.,0.));
#4558=DIRECTION('center_axis',(0.,-1.,0.));
#4559=DIRECTION('ref_axis',(1.,0.,0.));
#4560=DIRECTION('center_axis',(0.,-1.,0.));
#4561=DIRECTION('ref_axis',(1.,0.,0.));
#4562=DIRECTION('',(0.,1.,0.));
#4563=DIRECTION('center_axis',(0.,1.,0.));
#4564=DIRECTION('ref_axis',(0.,0.,1.));
#4565=DIRECTION('center_axis',(0.,-1.,0.));
#4566=DIRECTION('ref_axis',(1.,0.,0.));
#4567=DIRECTION('center_axis',(0.,-1.,0.));
#4568=DIRECTION('ref_axis',(1.,0.,0.));
#4569=DIRECTION('center_axis',(0.,-1.,0.));
#4570=DIRECTION('ref_axis',(1.,0.,0.));
#4571=DIRECTION('center_axis',(0.,-1.,0.));
#4572=DIRECTION('ref_axis',(1.,0.,0.));
#4573=DIRECTION('',(0.707106781186548,0.707106781186547,8.65956056235494E-17));
#4574=DIRECTION('center_axis',(0.,-1.,0.));
#4575=DIRECTION('ref_axis',(1.,0.,0.));
#4576=DIRECTION('center_axis',(0.,-1.,0.));
#4577=DIRECTION('ref_axis',(1.,0.,0.));
#4578=DIRECTION('',(0.,1.,0.));
#4579=DIRECTION('center_axis',(0.,1.,0.));
#4580=DIRECTION('ref_axis',(1.,0.,0.));
#4581=DIRECTION('center_axis',(0.,-1.,0.));
#4582=DIRECTION('ref_axis',(1.,0.,0.));
#4583=DIRECTION('',(-0.707106781186548,0.707106781186547,-8.65956056235494E-17));
#4584=DIRECTION('center_axis',(0.,-1.,0.));
#4585=DIRECTION('ref_axis',(0.,0.,-1.));
#4586=DIRECTION('center_axis',(0.,-1.,0.));
#4587=DIRECTION('ref_axis',(1.,0.,0.));
#4588=DIRECTION('',(0.,1.,0.));
#4589=DIRECTION('axis',(0.,0.,1.));
#4590=DIRECTION('refdir',(1.,0.,0.));
#4591=DIRECTION('center_axis',(0.,0.,1.));
#4592=DIRECTION('ref_axis',(1.,0.,0.));
#4593=DIRECTION('center_axis',(1.22464679914735E-16,-1.,0.));
#4594=DIRECTION('ref_axis',(-1.,-1.22464679914735E-16,0.));
#4595=DIRECTION('center_axis',(0.707106781186548,0.,0.707106781186548));
#4596=DIRECTION('ref_axis',(0.707106781186548,0.,-0.707106781186548));
#4597=DIRECTION('center_axis',(8.65956056235494E-17,-1.,-8.65956056235493E-17));
#4598=DIRECTION('ref_axis',(-0.707106781186547,-1.22464679914735E-16,0.707106781186547));
#4599=DIRECTION('center_axis',(1.,0.,0.));
#4600=DIRECTION('ref_axis',(6.12323399573676E-17,0.,-1.));
#4601=DIRECTION('center_axis',(7.49879891330929E-33,-1.,-1.22464679914735E-16));
#4602=DIRECTION('ref_axis',(-6.12323399573676E-17,-1.22464679914735E-16,
1.));
#4603=DIRECTION('center_axis',(0.707106781186548,0.,-0.707106781186548));
#4604=DIRECTION('ref_axis',(-0.707106781186548,0.,-0.707106781186548));
#4605=DIRECTION('center_axis',(-8.65956056235493E-17,-1.,-8.65956056235494E-17));
#4606=DIRECTION('ref_axis',(0.707106781186547,-1.22464679914735E-16,0.707106781186547));
#4607=DIRECTION('center_axis',(0.,0.,-1.));
#4608=DIRECTION('ref_axis',(-1.,0.,-1.22464679914735E-16));
#4609=DIRECTION('center_axis',(-1.22464679914735E-16,-1.,-1.49975978266186E-32));
#4610=DIRECTION('ref_axis',(1.,-1.22464679914735E-16,1.22464679914735E-16));
#4611=DIRECTION('center_axis',(-0.707106781186547,0.,-0.707106781186548));
#4612=DIRECTION('ref_axis',(-0.707106781186548,0.,0.707106781186547));
#4613=DIRECTION('center_axis',(-8.65956056235493E-17,-1.,8.65956056235493E-17));
#4614=DIRECTION('ref_axis',(0.707106781186548,-1.22464679914735E-16,-0.707106781186547));
#4615=DIRECTION('center_axis',(-1.,0.,0.));
#4616=DIRECTION('ref_axis',(-1.83697019872103E-16,0.,1.));
#4617=DIRECTION('center_axis',(-2.24963967399279E-32,-1.,1.22464679914735E-16));
#4618=DIRECTION('ref_axis',(1.83697019872103E-16,-1.22464679914735E-16,
-1.));
#4619=DIRECTION('center_axis',(-0.707106781186548,0.,0.707106781186548));
#4620=DIRECTION('ref_axis',(0.707106781186547,0.,0.707106781186548));
#4621=DIRECTION('center_axis',(8.65956056235493E-17,-1.,8.65956056235493E-17));
#4622=DIRECTION('ref_axis',(-0.707106781186547,-1.22464679914735E-16,-0.707106781186548));
#4623=DIRECTION('axis',(0.,0.,1.));
#4624=DIRECTION('refdir',(1.,0.,0.));
#4625=DIRECTION('center_axis',(0.,0.,1.));
#4626=DIRECTION('ref_axis',(1.,0.,0.));
#4627=DIRECTION('center_axis',(0.,-1.,0.));
#4628=DIRECTION('ref_axis',(0.,0.,-1.));
#4629=DIRECTION('center_axis',(0.,-1.,0.));
#4630=DIRECTION('ref_axis',(0.,0.,-1.));
#4631=DIRECTION('center_axis',(0.,1.,0.));
#4632=DIRECTION('ref_axis',(1.,0.,0.));
#4633=DIRECTION('center_axis',(0.,1.,0.));
#4634=DIRECTION('ref_axis',(1.,0.,0.));
#4635=DIRECTION('center_axis',(0.,1.,0.));
#4636=DIRECTION('ref_axis',(1.,0.,0.));
#4637=DIRECTION('center_axis',(0.,1.,0.));
#4638=DIRECTION('ref_axis',(1.,0.,0.));
#4639=DIRECTION('',(0.,-1.,0.));
#4640=DIRECTION('center_axis',(0.,-1.,0.));
#4641=DIRECTION('ref_axis',(1.,0.,0.));
#4642=DIRECTION('center_axis',(0.,1.,0.));
#4643=DIRECTION('ref_axis',(1.,0.,0.));
#4644=DIRECTION('center_axis',(0.,1.,0.));
#4645=DIRECTION('ref_axis',(1.,0.,0.));
#4646=DIRECTION('center_axis',(0.,1.,0.));
#4647=DIRECTION('ref_axis',(1.,0.,0.));
#4648=DIRECTION('center_axis',(0.,1.,0.));
#4649=DIRECTION('ref_axis',(1.,0.,0.));
#4650=DIRECTION('center_axis',(0.,1.,0.));
#4651=DIRECTION('ref_axis',(1.,0.,0.));
#4652=DIRECTION('center_axis',(0.,1.,0.));
#4653=DIRECTION('ref_axis',(1.,0.,0.));
#4654=DIRECTION('center_axis',(0.,-1.,0.));
#4655=DIRECTION('ref_axis',(1.,0.,0.));
#4656=DIRECTION('center_axis',(0.,-1.,0.));
#4657=DIRECTION('ref_axis',(0.,0.,-1.));
#4658=DIRECTION('center_axis',(6.12323399573677E-17,0.,1.));
#4659=DIRECTION('ref_axis',(1.,0.,0.));
#4660=DIRECTION('center_axis',(0.,-1.,0.));
#4661=DIRECTION('ref_axis',(0.,0.,-1.));
#4662=DIRECTION('center_axis',(0.,1.,0.));
#4663=DIRECTION('ref_axis',(1.,0.,0.));
#4664=DIRECTION('center_axis',(0.,-1.,0.));
#4665=DIRECTION('ref_axis',(1.,0.,0.));
#4666=DIRECTION('center_axis',(0.,-1.,0.));
#4667=DIRECTION('ref_axis',(0.,0.,-1.));
#4668=DIRECTION('center_axis',(0.,0.,1.));
#4669=DIRECTION('ref_axis',(1.,0.,0.));
#4670=DIRECTION('center_axis',(0.,-1.,0.));
#4671=DIRECTION('ref_axis',(0.,0.,-1.));
#4672=DIRECTION('center_axis',(0.,1.,0.));
#4673=DIRECTION('ref_axis',(1.,0.,0.));
#4674=DIRECTION('center_axis',(0.,-1.,0.));
#4675=DIRECTION('ref_axis',(1.,0.,0.));
#4676=DIRECTION('center_axis',(0.,-1.,0.));
#4677=DIRECTION('ref_axis',(0.,0.,-1.));
#4678=DIRECTION('center_axis',(0.,0.,1.));
#4679=DIRECTION('ref_axis',(1.,0.,0.));
#4680=DIRECTION('center_axis',(0.,-1.,0.));
#4681=DIRECTION('ref_axis',(0.,0.,-1.));
#4682=DIRECTION('center_axis',(0.,1.,0.));
#4683=DIRECTION('ref_axis',(1.,0.,0.));
#4684=DIRECTION('center_axis',(0.,-1.,0.));
#4685=DIRECTION('ref_axis',(1.,0.,0.));
#4686=DIRECTION('center_axis',(0.,-1.,0.));
#4687=DIRECTION('ref_axis',(0.,0.,-1.));
#4688=DIRECTION('center_axis',(0.,0.,1.));
#4689=DIRECTION('ref_axis',(1.,0.,0.));
#4690=DIRECTION('center_axis',(0.,-1.,0.));
#4691=DIRECTION('ref_axis',(0.,0.,-1.));
#4692=DIRECTION('center_axis',(0.,1.,0.));
#4693=DIRECTION('ref_axis',(1.,0.,0.));
#4694=DIRECTION('center_axis',(0.,-1.,0.));
#4695=DIRECTION('ref_axis',(1.,0.,0.));
#4696=DIRECTION('center_axis',(0.,-1.,0.));
#4697=DIRECTION('ref_axis',(0.,0.,-1.));
#4698=DIRECTION('center_axis',(6.12323399573676E-17,0.,1.));
#4699=DIRECTION('ref_axis',(1.,0.,0.));
#4700=DIRECTION('center_axis',(0.,-1.,0.));
#4701=DIRECTION('ref_axis',(0.,0.,-1.));
#4702=DIRECTION('center_axis',(0.,1.,0.));
#4703=DIRECTION('ref_axis',(1.,0.,0.));
#4704=DIRECTION('center_axis',(0.,-1.,0.));
#4705=DIRECTION('ref_axis',(1.,0.,0.));
#4706=DIRECTION('center_axis',(0.,-1.,0.));
#4707=DIRECTION('ref_axis',(0.,0.,-1.));
#4708=DIRECTION('center_axis',(0.,0.,1.));
#4709=DIRECTION('ref_axis',(1.,0.,0.));
#4710=DIRECTION('center_axis',(0.,-1.,0.));
#4711=DIRECTION('ref_axis',(0.,0.,-1.));
#4712=DIRECTION('center_axis',(0.,1.,0.));
#4713=DIRECTION('ref_axis',(1.,0.,0.));
#4714=DIRECTION('center_axis',(0.,1.,0.));
#4715=DIRECTION('ref_axis',(1.,0.,0.));
#4716=DIRECTION('',(0.,1.,0.));
#4717=DIRECTION('center_axis',(0.,-1.,0.));
#4718=DIRECTION('ref_axis',(1.,0.,0.));
#4719=DIRECTION('center_axis',(0.,-1.,0.));
#4720=DIRECTION('ref_axis',(1.,0.,0.));
#4721=DIRECTION('center_axis',(0.,1.,0.));
#4722=DIRECTION('ref_axis',(1.,0.,0.));
#4723=DIRECTION('center_axis',(0.,-1.,0.));
#4724=DIRECTION('ref_axis',(0.,0.,-1.));
#4725=DIRECTION('center_axis',(0.,0.,1.));
#4726=DIRECTION('ref_axis',(1.,0.,0.));
#4727=DIRECTION('center_axis',(0.,-1.,0.));
#4728=DIRECTION('ref_axis',(0.,0.,-1.));
#4729=DIRECTION('center_axis',(0.,-1.,0.));
#4730=DIRECTION('ref_axis',(-1.,0.,0.));
#4731=DIRECTION('center_axis',(0.,1.,0.));
#4732=DIRECTION('ref_axis',(1.,0.,0.));
#4733=DIRECTION('axis',(0.,0.,1.));
#4734=DIRECTION('refdir',(1.,0.,0.));
#4735=DIRECTION('center_axis',(0.,1.,0.));
#4736=DIRECTION('ref_axis',(0.,0.,1.));
#4737=DIRECTION('center_axis',(0.,-1.,0.));
#4738=DIRECTION('ref_axis',(1.,0.,0.));
#4739=DIRECTION('center_axis',(0.,-1.,0.));
#4740=DIRECTION('ref_axis',(1.,0.,0.));
#4741=DIRECTION('center_axis',(0.,-1.,0.));
#4742=DIRECTION('ref_axis',(1.,0.,0.));
#4743=DIRECTION('center_axis',(0.,-1.,0.));
#4744=DIRECTION('ref_axis',(1.,0.,0.));
#4745=DIRECTION('',(0.,1.,0.));
#4746=DIRECTION('center_axis',(0.,-1.,0.));
#4747=DIRECTION('ref_axis',(0.,0.,-1.));
#4748=DIRECTION('center_axis',(0.,-1.,0.));
#4749=DIRECTION('ref_axis',(1.,0.,0.));
#4750=DIRECTION('center_axis',(0.,-1.,0.));
#4751=DIRECTION('ref_axis',(1.,0.,0.));
#4752=DIRECTION('',(0.,1.,0.));
#4753=DIRECTION('center_axis',(0.,1.,0.));
#4754=DIRECTION('ref_axis',(0.,0.,1.));
#4755=DIRECTION('center_axis',(0.,-1.,0.));
#4756=DIRECTION('ref_axis',(1.,0.,0.));
#4757=DIRECTION('center_axis',(0.,-1.,0.));
#4758=DIRECTION('ref_axis',(1.,0.,0.));
#4759=DIRECTION('center_axis',(0.,-1.,0.));
#4760=DIRECTION('ref_axis',(1.,0.,0.));
#4761=DIRECTION('center_axis',(0.,-1.,0.));
#4762=DIRECTION('ref_axis',(1.,0.,0.));
#4763=DIRECTION('',(0.,1.,0.));
#4764=DIRECTION('center_axis',(0.,-1.,0.));
#4765=DIRECTION('ref_axis',(0.,0.,-1.));
#4766=DIRECTION('center_axis',(0.,-1.,0.));
#4767=DIRECTION('ref_axis',(1.,0.,0.));
#4768=DIRECTION('center_axis',(0.,-1.,0.));
#4769=DIRECTION('ref_axis',(1.,0.,0.));
#4770=DIRECTION('',(0.,1.,0.));
#4771=DIRECTION('',(0.,0.,1.));
#4772=DIRECTION('',(1.,0.,0.));
#4773=DIRECTION('',(0.,0.,1.));
#4774=DIRECTION('',(1.,0.,0.));
#4775=DIRECTION('',(0.,0.,1.));
#4776=DIRECTION('',(1.,0.,0.));
#4777=DIRECTION('',(0.,0.,1.));
#4778=DIRECTION('',(1.,0.,0.));
#4779=DIRECTION('',(0.,0.,1.));
#4780=DIRECTION('',(1.,0.,0.));
#4781=DIRECTION('axis',(0.,0.,1.));
#4782=DIRECTION('refdir',(1.,0.,0.));
#4783=DIRECTION('center_axis',(0.,0.,1.));
#4784=DIRECTION('ref_axis',(1.,0.,0.));
#4785=DIRECTION('center_axis',(0.,0.,1.));
#4786=DIRECTION('ref_axis',(1.,0.,0.));
#4787=DIRECTION('',(0.,0.,1.));
#4788=DIRECTION('center_axis',(0.,0.,-1.));
#4789=DIRECTION('ref_axis',(1.,0.,0.));
#4790=DIRECTION('center_axis',(0.,0.,1.));
#4791=DIRECTION('ref_axis',(1.,0.,0.));
#4792=DIRECTION('center_axis',(0.,0.,1.));
#4793=DIRECTION('ref_axis',(1.,0.,0.));
#4794=DIRECTION('center_axis',(0.,0.,1.));
#4795=DIRECTION('ref_axis',(1.,0.,0.));
#4796=DIRECTION('center_axis',(0.,0.,1.));
#4797=DIRECTION('ref_axis',(1.,0.,0.));
#4798=DIRECTION('',(0.,0.,1.));
#4799=DIRECTION('center_axis',(0.,0.,-1.));
#4800=DIRECTION('ref_axis',(1.,0.,0.));
#4801=DIRECTION('center_axis',(0.,0.,1.));
#4802=DIRECTION('ref_axis',(1.,0.,0.));
#4803=DIRECTION('center_axis',(0.,0.,1.));
#4804=DIRECTION('ref_axis',(1.,0.,0.));
#4805=DIRECTION('center_axis',(0.,0.,1.));
#4806=DIRECTION('ref_axis',(1.,0.,0.));
#4807=DIRECTION('center_axis',(0.,0.,1.));
#4808=DIRECTION('ref_axis',(1.,0.,0.));
#4809=DIRECTION('',(0.,0.,1.));
#4810=DIRECTION('center_axis',(0.,0.,-1.));
#4811=DIRECTION('ref_axis',(1.,0.,0.));
#4812=DIRECTION('center_axis',(0.,0.,1.));
#4813=DIRECTION('ref_axis',(1.,0.,0.));
#4814=DIRECTION('center_axis',(0.,0.,1.));
#4815=DIRECTION('ref_axis',(1.,0.,0.));
#4816=DIRECTION('center_axis',(0.,0.,1.));
#4817=DIRECTION('ref_axis',(1.,0.,0.));
#4818=DIRECTION('center_axis',(0.,0.,1.));
#4819=DIRECTION('ref_axis',(1.,0.,0.));
#4820=DIRECTION('',(0.,0.,1.));
#4821=DIRECTION('center_axis',(0.,0.,-1.));
#4822=DIRECTION('ref_axis',(1.,0.,0.));
#4823=DIRECTION('center_axis',(0.,0.,1.));
#4824=DIRECTION('ref_axis',(1.,0.,0.));
#4825=DIRECTION('center_axis',(0.,0.,1.));
#4826=DIRECTION('ref_axis',(1.,0.,0.));
#4827=DIRECTION('center_axis',(0.,0.,1.));
#4828=DIRECTION('ref_axis',(1.,0.,0.));
#4829=DIRECTION('center_axis',(0.,0.,1.));
#4830=DIRECTION('ref_axis',(1.,0.,0.));
#4831=DIRECTION('',(0.,0.,1.));
#4832=DIRECTION('center_axis',(0.,0.,1.));
#4833=DIRECTION('ref_axis',(1.,0.,0.));
#4834=DIRECTION('center_axis',(0.,0.,1.));
#4835=DIRECTION('ref_axis',(1.,0.,0.));
#4836=DIRECTION('',(0.,0.,1.));
#4837=DIRECTION('center_axis',(0.,0.,1.));
#4838=DIRECTION('ref_axis',(1.,0.,0.));
#4839=DIRECTION('center_axis',(0.,0.,1.));
#4840=DIRECTION('ref_axis',(1.,0.,0.));
#4841=DIRECTION('',(0.,0.,1.));
#4842=DIRECTION('center_axis',(0.,0.,1.));
#4843=DIRECTION('ref_axis',(1.,0.,0.));
#4844=DIRECTION('center_axis',(0.,0.,1.));
#4845=DIRECTION('ref_axis',(1.,0.,0.));
#4846=DIRECTION('',(0.,0.,1.));
#4847=DIRECTION('center_axis',(0.,0.,1.));
#4848=DIRECTION('ref_axis',(1.,0.,0.));
#4849=DIRECTION('center_axis',(0.,0.,1.));
#4850=DIRECTION('ref_axis',(1.,0.,0.));
#4851=DIRECTION('',(0.,0.,-1.));
#4852=DIRECTION('center_axis',(0.,0.,1.));
#4853=DIRECTION('ref_axis',(1.,0.,0.));
#4854=DIRECTION('center_axis',(0.,0.,1.));
#4855=DIRECTION('ref_axis',(1.,0.,0.));
#4856=DIRECTION('center_axis',(0.,0.,-1.));
#4857=DIRECTION('ref_axis',(1.,0.,0.));
#4858=DIRECTION('center_axis',(0.,0.,1.));
#4859=DIRECTION('ref_axis',(1.,0.,0.));
#4860=DIRECTION('center_axis',(0.,0.,-1.));
#4861=DIRECTION('ref_axis',(1.,0.,0.));
#4862=DIRECTION('',(0.,0.,-1.));
#4863=DIRECTION('center_axis',(0.,0.,1.));
#4864=DIRECTION('ref_axis',(1.,0.,0.));
#4865=DIRECTION('center_axis',(0.,0.,1.));
#4866=DIRECTION('ref_axis',(1.,0.,0.));
#4867=DIRECTION('',(0.,0.,-1.));
#4868=DIRECTION('center_axis',(0.,0.,1.));
#4869=DIRECTION('ref_axis',(1.,0.,0.));
#4870=DIRECTION('center_axis',(0.,0.,1.));
#4871=DIRECTION('ref_axis',(1.,0.,0.));
#4872=DIRECTION('center_axis',(0.,0.,1.));
#4873=DIRECTION('ref_axis',(1.,0.,0.));
#4874=DIRECTION('axis',(0.,0.,1.));
#4875=DIRECTION('refdir',(1.,0.,0.));
#4876=DIRECTION('center_axis',(0.866025403784439,0.,-0.5));
#4877=DIRECTION('ref_axis',(0.5,0.,0.866025403784439));
#4878=DIRECTION('',(-0.5,0.,-0.866025403784439));
#4879=DIRECTION('',(0.,-1.,0.));
#4880=DIRECTION('',(0.5,0.,0.866025403784439));
#4881=DIRECTION('',(0.,-1.,0.));
#4882=DIRECTION('center_axis',(1.60246890531964E-16,0.,-1.));
#4883=DIRECTION('ref_axis',(1.,0.,1.60246890531964E-16));
#4884=DIRECTION('',(-1.,0.,-1.60246890531964E-16));
#4885=DIRECTION('',(0.,-1.,0.));
#4886=DIRECTION('',(1.,0.,1.60246890531964E-16));
#4887=DIRECTION('center_axis',(-0.866025403784439,0.,-0.5));
#4888=DIRECTION('ref_axis',(0.5,0.,-0.866025403784439));
#4889=DIRECTION('',(-0.5,0.,0.866025403784439));
#4890=DIRECTION('',(0.,-1.,0.));
#4891=DIRECTION('',(0.5,0.,-0.866025403784439));
#4892=DIRECTION('center_axis',(-0.866025403784439,0.,0.5));
#4893=DIRECTION('ref_axis',(-0.5,0.,-0.866025403784439));
#4894=DIRECTION('',(0.5,0.,0.866025403784439));
#4895=DIRECTION('',(0.,-1.,0.));
#4896=DIRECTION('',(-0.5,0.,-0.866025403784439));
#4897=DIRECTION('center_axis',(-1.60246890531964E-16,0.,1.));
#4898=DIRECTION('ref_axis',(-1.,0.,-1.60246890531964E-16));
#4899=DIRECTION('',(1.,0.,1.60246890531964E-16));
#4900=DIRECTION('',(0.,-1.,0.));
#4901=DIRECTION('',(-1.,0.,-1.60246890531964E-16));
#4902=DIRECTION('center_axis',(0.866025403784439,0.,0.5));
#4903=DIRECTION('ref_axis',(-0.5,0.,0.866025403784439));
#4904=DIRECTION('',(0.5,0.,-0.866025403784439));
#4905=DIRECTION('',(-0.5,0.,0.866025403784439));
#4906=DIRECTION('center_axis',(0.,1.,0.));
#4907=DIRECTION('ref_axis',(1.,0.,0.));
#4908=DIRECTION('center_axis',(0.,-1.,0.));
#4909=DIRECTION('ref_axis',(0.,0.,-1.));
#4910=DIRECTION('center_axis',(0.,1.,0.));
#4911=DIRECTION('ref_axis',(1.,0.,0.));
#4912=DIRECTION('center_axis',(0.,1.,0.));
#4913=DIRECTION('ref_axis',(1.,0.,0.));
#4914=DIRECTION('center_axis',(0.,1.,0.));
#4915=DIRECTION('ref_axis',(0.,0.,1.));
#4916=DIRECTION('center_axis',(0.,-1.,0.));
#4917=DIRECTION('ref_axis',(1.,0.,0.));
#4918=DIRECTION('center_axis',(0.,-1.,0.));
#4919=DIRECTION('ref_axis',(1.,0.,0.));
#4920=DIRECTION('center_axis',(0.,-1.,0.));
#4921=DIRECTION('ref_axis',(1.,0.,0.));
#4922=DIRECTION('',(0.707106781186547,0.707106781186548,8.65956056235493E-17));
#4923=DIRECTION('center_axis',(0.,-1.,0.));
#4924=DIRECTION('ref_axis',(1.,0.,0.));
#4925=DIRECTION('center_axis',(0.,-1.,0.));
#4926=DIRECTION('ref_axis',(1.,0.,0.));
#4927=DIRECTION('',(0.,1.,0.));
#4928=DIRECTION('center_axis',(0.,1.,0.));
#4929=DIRECTION('ref_axis',(1.,0.,0.));
#4930=DIRECTION('center_axis',(0.,-1.,0.));
#4931=DIRECTION('ref_axis',(1.,0.,0.));
#4932=DIRECTION('',(-0.707106781186547,0.707106781186548,-8.65956056235493E-17));
#4933=DIRECTION('center_axis',(0.,-1.,0.));
#4934=DIRECTION('ref_axis',(0.,0.,-1.));
#4935=DIRECTION('center_axis',(0.,-1.,0.));
#4936=DIRECTION('ref_axis',(1.,0.,0.));
#4937=DIRECTION('center_axis',(0.,1.,0.));
#4938=DIRECTION('ref_axis',(1.,0.,0.));
#4939=DIRECTION('center_axis',(0.,1.,0.));
#4940=DIRECTION('ref_axis',(1.,0.,0.));
#4941=DIRECTION('',(-0.447213595499958,0.894427190999916,-5.47678698264203E-17));
#4942=DIRECTION('center_axis',(0.,-1.,0.));
#4943=DIRECTION('ref_axis',(1.,0.,0.));
#4944=DIRECTION('',(0.,1.,0.));
#4945=DIRECTION('',(0.,0.,1.));
#4946=DIRECTION('',(1.,0.,0.));
#4947=DIRECTION('',(0.,0.,1.));
#4948=DIRECTION('',(1.,0.,0.));
#4949=DIRECTION('',(0.,0.,1.));
#4950=DIRECTION('',(1.,0.,0.));
#4951=DIRECTION('',(0.,-1.,2.22044604925031E-16));
#4952=DIRECTION('',(1.,0.,0.));
#4953=DIRECTION('',(0.,-1.,2.22044604925031E-16));
#4954=DIRECTION('',(1.,0.,0.));
#4955=DIRECTION('',(0.,-1.,2.22044604925031E-16));
#4956=DIRECTION('',(1.,0.,0.));
#4957=DIRECTION('',(0.,-1.,2.22044604925031E-16));
#4958=DIRECTION('',(1.,0.,0.));
#4959=DIRECTION('',(0.,-1.,2.22044604925031E-16));
#4960=DIRECTION('',(1.,0.,0.));
#4961=DIRECTION('',(0.,-1.,2.22044604925031E-16));
#4962=DIRECTION('',(1.,0.,0.));
#4963=DIRECTION('',(0.,-1.,2.22044604925031E-16));
#4964=DIRECTION('',(1.,0.,0.));
#4965=DIRECTION('',(0.,-1.,2.22044604925031E-16));
#4966=DIRECTION('',(1.,0.,0.));
#4967=DIRECTION('',(0.,-1.,2.22044604925031E-16));
#4968=DIRECTION('',(1.,0.,0.));
#4969=DIRECTION('',(0.,0.,1.));
#4970=DIRECTION('',(1.,0.,0.));
#4971=DIRECTION('',(0.,0.,1.));
#4972=DIRECTION('',(1.,0.,0.));
#4973=DIRECTION('',(0.,-1.,2.22044604925031E-16));
#4974=DIRECTION('',(1.,0.,0.));
#4975=DIRECTION('',(0.,-1.,2.22044604925031E-16));
#4976=DIRECTION('',(1.,0.,0.));
#4977=DIRECTION('',(0.,-1.,2.22044604925031E-16));
#4978=DIRECTION('',(1.,0.,0.));
#4979=DIRECTION('',(0.,-1.,2.22044604925031E-16));
#4980=DIRECTION('',(1.,0.,0.));
#4981=DIRECTION('',(0.,-1.,2.22044604925031E-16));
#4982=DIRECTION('',(1.,0.,0.));
#4983=DIRECTION('',(0.,-1.,2.22044604925031E-16));
#4984=DIRECTION('',(1.,0.,0.));
#4985=DIRECTION('',(0.,-1.,2.22044604925031E-16));
#4986=DIRECTION('',(1.,0.,0.));
#4987=DIRECTION('',(0.,-1.,2.22044604925031E-16));
#4988=DIRECTION('',(1.,0.,0.));
#4989=DIRECTION('',(0.,-1.,2.22044604925031E-16));
#4990=DIRECTION('',(1.,0.,0.));
#4991=DIRECTION('axis',(0.,0.,1.));
#4992=DIRECTION('refdir',(1.,0.,0.));
#4993=DIRECTION('axis',(0.,0.,1.));
#4994=DIRECTION('refdir',(1.,0.,0.));
#4995=DIRECTION('center_axis',(0.,0.,1.));
#4996=DIRECTION('ref_axis',(1.,0.,0.));
#4997=DIRECTION('',(0.,0.,-1.));
#4998=DIRECTION('center_axis',(0.,0.,1.));
#4999=DIRECTION('ref_axis',(1.,0.,0.));
#5000=DIRECTION('',(0.,0.,1.));
#5001=DIRECTION('center_axis',(0.,0.,1.));
#5002=DIRECTION('ref_axis',(1.,0.,0.));
#5003=DIRECTION('center_axis',(0.,1.,0.));
#5004=DIRECTION('ref_axis',(-1.,0.,0.));
#5005=DIRECTION('',(1.,0.,0.));
#5006=DIRECTION('',(0.,0.,-1.));
#5007=DIRECTION('',(-1.,0.,0.));
#5008=DIRECTION('center_axis',(0.,0.,1.));
#5009=DIRECTION('ref_axis',(1.,0.,0.));
#5010=DIRECTION('',(-1.,0.,0.));
#5011=DIRECTION('center_axis',(0.,0.,1.));
#5012=DIRECTION('ref_axis',(1.,0.,0.));
#5013=DIRECTION('center_axis',(0.,0.,1.));
#5014=DIRECTION('ref_axis',(1.,0.,0.));
#5015=DIRECTION('center_axis',(0.,0.,1.));
#5016=DIRECTION('ref_axis',(1.,0.,0.));
#5017=DIRECTION('center_axis',(0.,0.,1.));
#5018=DIRECTION('ref_axis',(1.,0.,0.));
#5019=DIRECTION('center_axis',(0.,0.,1.));
#5020=DIRECTION('ref_axis',(1.,0.,0.));
#5021=DIRECTION('center_axis',(0.,0.,-1.));
#5022=DIRECTION('ref_axis',(1.,0.,0.));
#5023=DIRECTION('center_axis',(0.,0.,1.));
#5024=DIRECTION('ref_axis',(1.,0.,0.));
#5025=DIRECTION('',(0.,0.,-1.));
#5026=DIRECTION('center_axis',(0.,0.,1.));
#5027=DIRECTION('ref_axis',(1.,0.,0.));
#5028=DIRECTION('',(0.,0.,-1.));
#5029=DIRECTION('center_axis',(0.,0.,1.));
#5030=DIRECTION('ref_axis',(1.,0.,0.));
#5031=DIRECTION('center_axis',(0.,0.,1.));
#5032=DIRECTION('ref_axis',(1.,0.,0.));
#5033=DIRECTION('center_axis',(0.,-1.,0.));
#5034=DIRECTION('ref_axis',(1.,0.,0.));
#5035=DIRECTION('',(1.,0.,0.));
#5036=DIRECTION('',(0.,0.,1.));
#5037=DIRECTION('center_axis',(0.,0.,1.));
#5038=DIRECTION('ref_axis',(-1.,1.22464679914735E-16,0.));
#5039=DIRECTION('center_axis',(0.,0.,1.));
#5040=DIRECTION('ref_axis',(1.,0.,0.));
#5041=DIRECTION('center_axis',(0.,0.,1.));
#5042=DIRECTION('ref_axis',(1.,0.,0.));
#5043=DIRECTION('center_axis',(0.,0.,1.));
#5044=DIRECTION('ref_axis',(1.,0.,0.));
#5045=DIRECTION('center_axis',(0.,0.,-1.));
#5046=DIRECTION('ref_axis',(1.,0.,0.));
#5047=DIRECTION('center_axis',(0.,0.,1.));
#5048=DIRECTION('ref_axis',(1.,0.,0.));
#5049=DIRECTION('',(0.,0.,-1.));
#5050=DIRECTION('center_axis',(0.,0.,1.));
#5051=DIRECTION('ref_axis',(1.,0.,0.));
#5052=DIRECTION('',(0.,0.,-1.));
#5053=DIRECTION('center_axis',(0.,0.,1.));
#5054=DIRECTION('ref_axis',(1.,0.,0.));
#5055=DIRECTION('center_axis',(0.,0.,1.));
#5056=DIRECTION('ref_axis',(1.,0.,0.));
#5057=DIRECTION('center_axis',(0.,0.,1.));
#5058=DIRECTION('ref_axis',(1.,0.,0.));
#5059=DIRECTION('axis',(0.,0.,1.));
#5060=DIRECTION('refdir',(1.,0.,0.));
#5061=DIRECTION('center_axis',(0.,0.,1.));
#5062=DIRECTION('ref_axis',(1.,0.,0.));
#5063=DIRECTION('center_axis',(0.,0.,-1.));
#5064=DIRECTION('ref_axis',(1.,0.,0.));
#5065=DIRECTION('',(0.,0.,-1.));
#5066=DIRECTION('center_axis',(0.,0.,-1.));
#5067=DIRECTION('ref_axis',(1.,0.,0.));
#5068=DIRECTION('center_axis',(0.,0.,1.));
#5069=DIRECTION('ref_axis',(1.,0.,0.));
#5070=DIRECTION('center_axis',(0.,0.,1.));
#5071=DIRECTION('ref_axis',(1.,0.,0.));
#5072=DIRECTION('',(0.,0.,-1.));
#5073=DIRECTION('center_axis',(0.,0.,1.));
#5074=DIRECTION('ref_axis',(1.,0.,0.));
#5075=DIRECTION('center_axis',(0.,0.,1.));
#5076=DIRECTION('ref_axis',(1.,0.,0.));
#5077=DIRECTION('center_axis',(0.,0.,1.));
#5078=DIRECTION('ref_axis',(1.,0.,0.));
#5079=DIRECTION('axis',(0.,0.,1.));
#5080=DIRECTION('refdir',(1.,0.,0.));
#5081=DIRECTION('center_axis',(1.,0.,0.));
#5082=DIRECTION('ref_axis',(0.,0.,-1.));
#5083=DIRECTION('',(0.,0.,1.));
#5084=DIRECTION('center_axis',(1.,0.,0.));
#5085=DIRECTION('ref_axis',(0.,0.,-1.));
#5086=DIRECTION('center_axis',(1.,0.,0.));
#5087=DIRECTION('ref_axis',(0.,0.,-1.));
#5088=DIRECTION('center_axis',(1.,0.,0.));
#5089=DIRECTION('ref_axis',(0.,0.,-1.));
#5090=DIRECTION('',(1.,0.,0.));
#5091=DIRECTION('center_axis',(1.,0.,0.));
#5092=DIRECTION('ref_axis',(0.,0.,-1.));
#5093=DIRECTION('',(0.,0.,-1.));
#5094=DIRECTION('center_axis',(0.,0.,1.));
#5095=DIRECTION('ref_axis',(1.,0.,0.));
#5096=DIRECTION('center_axis',(0.,0.,-1.));
#5097=DIRECTION('ref_axis',(1.,0.,0.));
#5098=DIRECTION('',(0.,0.,-1.));
#5099=DIRECTION('center_axis',(0.,0.,-1.));
#5100=DIRECTION('ref_axis',(1.,0.,0.));
#5101=DIRECTION('center_axis',(0.,0.,1.));
#5102=DIRECTION('ref_axis',(1.,0.,0.));
#5103=DIRECTION('center_axis',(0.,0.,1.));
#5104=DIRECTION('ref_axis',(1.,0.,0.));
#5105=DIRECTION('',(0.,0.,-1.));
#5106=DIRECTION('center_axis',(0.,0.,1.));
#5107=DIRECTION('ref_axis',(1.,0.,0.));
#5108=DIRECTION('center_axis',(0.,0.,1.));
#5109=DIRECTION('ref_axis',(1.,0.,0.));
#5110=DIRECTION('center_axis',(0.,0.,1.));
#5111=DIRECTION('ref_axis',(1.,0.,0.));
#5112=DIRECTION('axis',(0.,0.,1.));
#5113=DIRECTION('refdir',(1.,0.,0.));
#5114=DIRECTION('center_axis',(0.,1.,0.));
#5115=DIRECTION('ref_axis',(1.,0.,0.));
#5116=DIRECTION('center_axis',(0.,1.,0.));
#5117=DIRECTION('ref_axis',(1.,0.,0.));
#5118=DIRECTION('center_axis',(0.866025403784439,0.,-0.5));
#5119=DIRECTION('ref_axis',(0.5,0.,0.866025403784439));
#5120=DIRECTION('',(0.5,0.,0.866025403784439));
#5121=DIRECTION('',(0.,-1.,0.));
#5122=DIRECTION('',(0.5,0.,0.866025403784439));
#5123=DIRECTION('',(0.,-1.,0.));
#5124=DIRECTION('center_axis',(1.20185167898973E-16,0.,-1.));
#5125=DIRECTION('ref_axis',(1.,0.,1.20185167898973E-16));
#5126=DIRECTION('',(1.,0.,1.20185167898973E-16));
#5127=DIRECTION('',(0.,-1.,0.));
#5128=DIRECTION('',(1.,0.,1.20185167898973E-16));
#5129=DIRECTION('center_axis',(-0.866025403784439,0.,-0.5));
#5130=DIRECTION('ref_axis',(0.5,0.,-0.866025403784439));
#5131=DIRECTION('',(0.5,0.,-0.866025403784439));
#5132=DIRECTION('',(0.,-1.,0.));
#5133=DIRECTION('',(0.5,0.,-0.866025403784439));
#5134=DIRECTION('center_axis',(-0.866025403784439,0.,0.5));
#5135=DIRECTION('ref_axis',(-0.5,0.,-0.866025403784439));
#5136=DIRECTION('',(-0.5,0.,-0.866025403784439));
#5137=DIRECTION('',(0.,-1.,0.));
#5138=DIRECTION('',(-0.5,0.,-0.866025403784439));
#5139=DIRECTION('center_axis',(-2.40370335797945E-16,0.,1.));
#5140=DIRECTION('ref_axis',(-1.,0.,-2.40370335797945E-16));
#5141=DIRECTION('',(-1.,0.,-2.40370335797945E-16));
#5142=DIRECTION('',(0.,-1.,0.));
#5143=DIRECTION('',(-1.,0.,-2.40370335797945E-16));
#5144=DIRECTION('center_axis',(0.866025403784439,0.,0.5));
#5145=DIRECTION('ref_axis',(-0.5,0.,0.866025403784439));
#5146=DIRECTION('',(-0.5,0.,0.866025403784439));
#5147=DIRECTION('',(-0.5,0.,0.866025403784439));
#5148=DIRECTION('center_axis',(0.,-1.,0.));
#5149=DIRECTION('ref_axis',(0.,0.,-1.));
#5150=DIRECTION('center_axis',(0.,1.,0.));
#5151=DIRECTION('ref_axis',(0.,0.,1.));
#5152=DIRECTION('center_axis',(0.,-1.,0.));
#5153=DIRECTION('ref_axis',(1.,0.,0.));
#5154=DIRECTION('center_axis',(0.,-1.,0.));
#5155=DIRECTION('ref_axis',(1.,0.,0.));
#5156=DIRECTION('center_axis',(0.,-1.,0.));
#5157=DIRECTION('ref_axis',(1.,0.,0.));
#5158=DIRECTION('',(0.707106781186548,0.707106781186547,8.65956056235494E-17));
#5159=DIRECTION('center_axis',(0.,-1.,0.));
#5160=DIRECTION('ref_axis',(1.,0.,0.));
#5161=DIRECTION('',(0.,1.,0.));
#5162=DIRECTION('',(0.,0.,1.));
#5163=DIRECTION('',(1.,0.,0.));
#5164=DIRECTION('',(0.,-1.,2.22044604925031E-16));
#5165=DIRECTION('',(1.,0.,0.));
#5166=DIRECTION('',(0.,0.,1.));
#5167=DIRECTION('',(1.,0.,0.));
#5168=DIRECTION('',(0.,-1.,2.22044604925031E-16));
#5169=DIRECTION('',(1.,0.,0.));
#5170=DIRECTION('',(0.,-1.,2.22044604925031E-16));
#5171=DIRECTION('',(1.,0.,0.));
#5172=DIRECTION('',(0.,-1.,2.22044604925031E-16));
#5173=DIRECTION('',(1.,0.,0.));
#5174=DIRECTION('',(0.,-1.,2.22044604925031E-16));
#5175=DIRECTION('',(1.,0.,0.));
#5176=DIRECTION('',(0.,0.,1.));
#5177=DIRECTION('',(1.,0.,0.));
#5178=DIRECTION('',(0.,0.,1.));
#5179=DIRECTION('',(1.,0.,0.));
#5180=DIRECTION('',(0.,0.,1.));
#5181=DIRECTION('',(2.22044604925031E-16,-1.,0.));
#5182=DIRECTION('',(0.,0.,1.));
#5183=DIRECTION('',(1.,0.,0.));
#5184=DIRECTION('',(0.,-1.,2.22044604925031E-16));
#5185=DIRECTION('',(1.,0.,0.));
#5186=DIRECTION('',(0.,0.,1.));
#5187=DIRECTION('',(1.,0.,0.));
#5188=DIRECTION('',(0.,-1.,2.22044604925031E-16));
#5189=DIRECTION('',(1.,0.,0.));
#5190=DIRECTION('',(0.,-1.,2.22044604925031E-16));
#5191=DIRECTION('',(1.,0.,0.));
#5192=DIRECTION('',(0.,-1.,2.22044604925031E-16));
#5193=DIRECTION('',(1.,0.,0.));
#5194=DIRECTION('',(0.,-1.,2.22044604925031E-16));
#5195=DIRECTION('',(1.,0.,0.));
#5196=DIRECTION('',(0.,0.,1.));
#5197=DIRECTION('',(1.,0.,0.));
#5198=DIRECTION('',(0.,0.,1.));
#5199=DIRECTION('',(1.,0.,0.));
#5200=DIRECTION('',(0.,0.,1.));
#5201=DIRECTION('',(2.22044604925031E-16,-1.,0.));
#5202=DIRECTION('',(0.,0.,1.));
#5203=DIRECTION('',(1.,0.,0.));
#5204=DIRECTION('',(0.,0.,1.));
#5205=DIRECTION('',(1.,0.,0.));
#5206=DIRECTION('',(0.,0.,1.));
#5207=DIRECTION('',(1.,0.,0.));
#5208=DIRECTION('',(0.,0.,1.));
#5209=DIRECTION('',(2.22044604925031E-16,-1.,0.));
#5210=DIRECTION('',(0.,0.,1.));
#5211=DIRECTION('',(1.,0.,0.));
#5212=DIRECTION('',(0.,0.,1.));
#5213=DIRECTION('',(1.,0.,0.));
#5214=DIRECTION('',(0.,0.,1.));
#5215=DIRECTION('',(2.22044604925031E-16,-1.,0.));
#5216=DIRECTION('',(0.,0.,1.));
#5217=DIRECTION('',(1.,0.,0.));
#5218=DIRECTION('',(6.12383218241995E-17,1.14683109657184E-32,1.));
#5219=DIRECTION('',(0.939691726438371,-0.342022600515334,-5.75451443591707E-17));
#5220=DIRECTION('',(6.12323399573676E-17,1.51666983120495E-33,1.));
#5221=DIRECTION('',(-0.906538190087682,-0.42212380874875,5.5509454639786E-17));
#5222=DIRECTION('',(1.22468315601198E-16,9.70789062592691E-33,1.));
#5223=DIRECTION('',(0.573127361470468,-0.819466306527547,-7.01899425842469E-17));
#5224=CARTESIAN_POINT('',(0.,0.,0.));
#5225=CARTESIAN_POINT('',(0.,0.,0.));
#5226=CARTESIAN_POINT('',(0.,0.,0.));
#5227=CARTESIAN_POINT('Origin',(6.23223304703363,-1.76776695296637,-0.1));
#5228=CARTESIAN_POINT('',(6.02223304703363,-1.76776695296637,0.));
#5229=CARTESIAN_POINT('Origin',(6.23223304703363,-1.76776695296637,0.));
#5230=CARTESIAN_POINT('',(6.02223304703363,-1.76776695296637,1.));
#5231=CARTESIAN_POINT('',(6.02223304703363,-1.76776695296637,-0.1));
#5232=CARTESIAN_POINT('Origin',(6.23223304703363,-1.76776695296637,1.));
#5233=CARTESIAN_POINT('Origin',(6.23223304703363,1.76776695296637,-0.1));
#5234=CARTESIAN_POINT('',(6.02223304703363,1.76776695296637,0.));
#5235=CARTESIAN_POINT('Origin',(6.23223304703363,1.76776695296637,0.));
#5236=CARTESIAN_POINT('',(6.02223304703363,1.76776695296637,1.));
#5237=CARTESIAN_POINT('',(6.02223304703363,1.76776695296637,-0.1));
#5238=CARTESIAN_POINT('Origin',(6.23223304703363,1.76776695296637,1.));
#5239=CARTESIAN_POINT('Origin',(9.76776695296637,1.76776695296637,-0.1));
#5240=CARTESIAN_POINT('',(9.55776695296637,1.76776695296637,0.));
#5241=CARTESIAN_POINT('Origin',(9.76776695296637,1.76776695296637,0.));
#5242=CARTESIAN_POINT('',(9.55776695296637,1.76776695296637,1.));
#5243=CARTESIAN_POINT('',(9.55776695296637,1.76776695296637,-0.1));
#5244=CARTESIAN_POINT('Origin',(9.76776695296637,1.76776695296637,1.));
#5245=CARTESIAN_POINT('Origin',(9.76776695296637,-1.76776695296637,-0.1));
#5246=CARTESIAN_POINT('',(9.55776695296637,-1.76776695296637,0.));
#5247=CARTESIAN_POINT('Origin',(9.76776695296637,-1.76776695296637,0.));
#5248=CARTESIAN_POINT('',(9.55776695296637,-1.76776695296637,1.));
#5249=CARTESIAN_POINT('',(9.55776695296637,-1.76776695296637,-0.1));
#5250=CARTESIAN_POINT('Origin',(9.76776695296637,-1.76776695296637,1.));
#5251=CARTESIAN_POINT('Origin',(-1.76776695296637,-1.76776695296637,-0.1));
#5252=CARTESIAN_POINT('',(-1.97776695296637,-1.76776695296637,0.));
#5253=CARTESIAN_POINT('Origin',(-1.76776695296637,-1.76776695296637,0.));
#5254=CARTESIAN_POINT('',(-1.97776695296637,-1.76776695296637,1.));
#5255=CARTESIAN_POINT('',(-1.97776695296637,-1.76776695296637,-0.1));
#5256=CARTESIAN_POINT('Origin',(-1.76776695296637,-1.76776695296637,1.));
#5257=CARTESIAN_POINT('Origin',(-1.76776695296637,1.76776695296637,-0.1));
#5258=CARTESIAN_POINT('',(-1.97776695296637,1.76776695296637,0.));
#5259=CARTESIAN_POINT('Origin',(-1.76776695296637,1.76776695296637,0.));
#5260=CARTESIAN_POINT('',(-1.97776695296637,1.76776695296637,1.));
#5261=CARTESIAN_POINT('',(-1.97776695296637,1.76776695296637,-0.1));
#5262=CARTESIAN_POINT('Origin',(-1.76776695296637,1.76776695296637,1.));
#5263=CARTESIAN_POINT('Origin',(1.76776695296637,1.76776695296637,-0.1));
#5264=CARTESIAN_POINT('',(1.55776695296637,1.76776695296637,0.));
#5265=CARTESIAN_POINT('Origin',(1.76776695296637,1.76776695296637,0.));
#5266=CARTESIAN_POINT('',(1.55776695296637,1.76776695296637,1.));
#5267=CARTESIAN_POINT('',(1.55776695296637,1.76776695296637,-0.1));
#5268=CARTESIAN_POINT('Origin',(1.76776695296637,1.76776695296637,1.));
#5269=CARTESIAN_POINT('Origin',(1.76776695296637,-1.76776695296637,-0.1));
#5270=CARTESIAN_POINT('',(1.55776695296637,-1.76776695296637,0.));
#5271=CARTESIAN_POINT('Origin',(1.76776695296637,-1.76776695296637,0.));
#5272=CARTESIAN_POINT('',(1.55776695296637,-1.76776695296637,1.));
#5273=CARTESIAN_POINT('',(1.55776695296637,-1.76776695296637,-0.1));
#5274=CARTESIAN_POINT('Origin',(1.76776695296637,-1.76776695296637,1.));
#5275=CARTESIAN_POINT('Origin',(11.5,6.5,0.));
#5276=CARTESIAN_POINT('',(11.5,6.5,0.));
#5277=CARTESIAN_POINT('',(-3.5,6.5,0.));
#5278=CARTESIAN_POINT('',(11.5,6.5,0.));
#5279=CARTESIAN_POINT('',(-3.5,6.5,1.));
#5280=CARTESIAN_POINT('',(-3.5,6.5,0.));
#5281=CARTESIAN_POINT('',(11.5,6.5,1.));
#5282=CARTESIAN_POINT('',(11.5,6.5,1.));
#5283=CARTESIAN_POINT('',(11.5,6.5,0.));
#5284=CARTESIAN_POINT('Origin',(11.5,-3.5,0.));
#5285=CARTESIAN_POINT('',(11.5,-3.5,0.));
#5286=CARTESIAN_POINT('',(11.5,-3.5,0.));
#5287=CARTESIAN_POINT('',(11.5,-3.5,1.));
#5288=CARTESIAN_POINT('',(11.5,-3.5,1.));
#5289=CARTESIAN_POINT('',(11.5,-3.5,0.));
#5290=CARTESIAN_POINT('Origin',(-3.5,-3.5,0.));
#5291=CARTESIAN_POINT('',(-3.5,-3.5,0.));
#5292=CARTESIAN_POINT('',(-3.5,-3.5,0.));
#5293=CARTESIAN_POINT('',(-3.5,-3.5,1.));
#5294=CARTESIAN_POINT('',(-3.5,-3.5,1.));
#5295=CARTESIAN_POINT('',(-3.5,-3.5,0.));
#5296=CARTESIAN_POINT('Origin',(-3.5,6.5,0.));
#5297=CARTESIAN_POINT('',(-3.5,6.5,0.));
#5298=CARTESIAN_POINT('',(-3.5,6.5,1.));
#5299=CARTESIAN_POINT('Origin',(4.,1.5,1.));
#5300=CARTESIAN_POINT('Origin',(4.,1.5,0.));
#5301=CARTESIAN_POINT('',(0.,0.,0.));
#5302=CARTESIAN_POINT('Origin',(0.9,0.,1.4));
#5303=CARTESIAN_POINT('',(0.988888264668966,0.25,1.4));
#5304=CARTESIAN_POINT('',(1.02,-1.18386380373883E-17,1.65));
#5305=CARTESIAN_POINT('Ctrl Pts',(0.988888264668966,0.25,1.4));
#5306=CARTESIAN_POINT('Ctrl Pts',(0.988888264668966,0.25,1.43153139415882));
#5307=CARTESIAN_POINT('Ctrl Pts',(0.990553370646674,0.243672048431404,1.46507214966317));
#5308=CARTESIAN_POINT('Ctrl Pts',(0.996491737296663,0.218119830014375,1.52662620974954));
#5309=CARTESIAN_POINT('Ctrl Pts',(1.00067109353237,0.198902128206072,1.5546512623872));
#5310=CARTESIAN_POINT('Ctrl Pts',(1.00845756932386,0.154654113568716,1.59889927702456));
#5311=CARTESIAN_POINT('Ctrl Pts',(1.01258144235289,0.126627870945253,1.61811920309393));
#5312=CARTESIAN_POINT('Ctrl Pts',(1.0183917429657,0.065069600391363,1.64367304400768));
#5313=CARTESIAN_POINT('Ctrl Pts',(1.02,0.031527330883376,1.65));
#5314=CARTESIAN_POINT('Ctrl Pts',(1.02,2.77555756156289E-17,1.65));
#5315=CARTESIAN_POINT('Ctrl Pts',(1.02,6.93889390390723E-18,1.65));
#5316=CARTESIAN_POINT('Ctrl Pts',(1.02,-0.031527330883376,1.65));
#5317=CARTESIAN_POINT('Ctrl Pts',(1.0183917429657,-0.065069600391363,1.64367304400768));
#5318=CARTESIAN_POINT('Ctrl Pts',(1.01258144235289,-0.126627870945253,1.61811920309393));
#5319=CARTESIAN_POINT('Ctrl Pts',(1.00845756932386,-0.154654113568716,1.59889927702456));
#5320=CARTESIAN_POINT('Ctrl Pts',(1.00067109353237,-0.198902128206072,1.5546512623872));
#5321=CARTESIAN_POINT('Ctrl Pts',(0.996491737296663,-0.218119830014375,
1.52662620974954));
#5322=CARTESIAN_POINT('Ctrl Pts',(0.990553370646674,-0.243672048431404,
1.46507214966317));
#5323=CARTESIAN_POINT('Ctrl Pts',(0.988888264668967,-0.25,1.43153139415882));
#5324=CARTESIAN_POINT('Ctrl Pts',(0.988888264668967,-0.25,1.36846860584118));
#5325=CARTESIAN_POINT('Ctrl Pts',(0.990553370646674,-0.243672048431404,
1.33492785033683));
#5326=CARTESIAN_POINT('Ctrl Pts',(0.996491737296663,-0.218119830014375,
1.27337379025046));
#5327=CARTESIAN_POINT('Ctrl Pts',(1.00067109353237,-0.198902128206072,1.2453487376128));
#5328=CARTESIAN_POINT('Ctrl Pts',(1.00845756932386,-0.154654113568716,1.20110072297544));
#5329=CARTESIAN_POINT('Ctrl Pts',(1.01258144235289,-0.126627870945254,1.18188079690607));
#5330=CARTESIAN_POINT('Ctrl Pts',(1.0183917429657,-0.0650696003913633,1.15632695599232));
#5331=CARTESIAN_POINT('Ctrl Pts',(1.02,-0.0315273308833761,1.15));
#5332=CARTESIAN_POINT('Ctrl Pts',(1.02,0.0315273308833759,1.15));
#5333=CARTESIAN_POINT('Ctrl Pts',(1.0183917429657,0.065069600391363,1.15632695599232));
#5334=CARTESIAN_POINT('Ctrl Pts',(1.01258144235289,0.126627870945253,1.18188079690607));
#5335=CARTESIAN_POINT('Ctrl Pts',(1.00845756932386,0.154654113568716,1.20110072297544));
#5336=CARTESIAN_POINT('Ctrl Pts',(1.00067109353237,0.198902128206072,1.2453487376128));
#5337=CARTESIAN_POINT('Ctrl Pts',(0.996491737296663,0.218119830014375,1.27337379025046));
#5338=CARTESIAN_POINT('Ctrl Pts',(0.990553370646674,0.243672048431404,1.33492785033683));
#5339=CARTESIAN_POINT('Ctrl Pts',(0.988888264668967,0.25,1.36846860584118));
#5340=CARTESIAN_POINT('Ctrl Pts',(0.988888264668967,0.25,1.4));
#5341=CARTESIAN_POINT('',(3.,-3.06161699786838E-17,1.65));
#5342=CARTESIAN_POINT('',(0.9,-3.06161699786838E-17,1.65));
#5343=CARTESIAN_POINT('',(2.98956518577535,0.25,1.4));
#5344=CARTESIAN_POINT('Ctrl Pts',(2.98956518577535,0.25,1.4));
#5345=CARTESIAN_POINT('Ctrl Pts',(2.98956518577535,0.25,1.36859378633186));
#5346=CARTESIAN_POINT('Ctrl Pts',(2.99011104995181,0.24372047740942,1.33510417960069));
#5347=CARTESIAN_POINT('Ctrl Pts',(2.99208145165098,0.218202539734559,1.27351367328886));
#5348=CARTESIAN_POINT('Ctrl Pts',(2.99347740802958,0.198964922639276,1.245411532046));
#5349=CARTESIAN_POINT('Ctrl Pts',(2.99609686518216,0.154588504271054,1.20103511367778));
#5350=CARTESIAN_POINT('Ctrl Pts',(2.99749070376198,0.126486346986081,1.18179746841036));
#5351=CARTESIAN_POINT('Ctrl Pts',(2.99945625936844,0.0648957875009219,1.15627950921557));
#5352=CARTESIAN_POINT('Ctrl Pts',(3.,0.0314061622633416,1.15));
#5353=CARTESIAN_POINT('Ctrl Pts',(3.,-0.0314061622633416,1.15));
#5354=CARTESIAN_POINT('Ctrl Pts',(2.99945625936844,-0.0648957875009221,
1.15627950921557));
#5355=CARTESIAN_POINT('Ctrl Pts',(2.99749070376198,-0.126486346986081,1.18179746841036));
#5356=CARTESIAN_POINT('Ctrl Pts',(2.99609686518216,-0.154588504271054,1.20103511367778));
#5357=CARTESIAN_POINT('Ctrl Pts',(2.99347740802958,-0.198964922639276,1.245411532046));
#5358=CARTESIAN_POINT('Ctrl Pts',(2.99208145165098,-0.218202539734559,1.27351367328886));
#5359=CARTESIAN_POINT('Ctrl Pts',(2.99011104995181,-0.24372047740942,1.33510417960069));
#5360=CARTESIAN_POINT('Ctrl Pts',(2.98956518577535,-0.25,1.36859378633186));
#5361=CARTESIAN_POINT('Ctrl Pts',(2.98956518577535,-0.25,1.43140621366814));
#5362=CARTESIAN_POINT('Ctrl Pts',(2.99011104995181,-0.24372047740942,1.4648958203993));
#5363=CARTESIAN_POINT('Ctrl Pts',(2.99208145165098,-0.21820253973456,1.52648632671114));
#5364=CARTESIAN_POINT('Ctrl Pts',(2.99347740802958,-0.198964922639276,1.554588467954));
#5365=CARTESIAN_POINT('Ctrl Pts',(2.99609686518216,-0.154588504271054,1.59896488632222));
#5366=CARTESIAN_POINT('Ctrl Pts',(2.99749070376198,-0.126486346986082,1.61820253158964));
#5367=CARTESIAN_POINT('Ctrl Pts',(2.99945625936844,-0.0648957875009221,
1.64372049078443));
#5368=CARTESIAN_POINT('Ctrl Pts',(3.,-0.0314061622633417,1.65));
#5369=CARTESIAN_POINT('Ctrl Pts',(3.,-5.55111512312578E-17,1.65));
#5370=CARTESIAN_POINT('Ctrl Pts',(3.,-2.08166817117217E-17,1.65));
#5371=CARTESIAN_POINT('Ctrl Pts',(3.,0.0314061622633416,1.65));
#5372=CARTESIAN_POINT('Ctrl Pts',(2.99945625936844,0.0648957875009221,1.64372049078443));
#5373=CARTESIAN_POINT('Ctrl Pts',(2.99749070376198,0.126486346986081,1.61820253158964));
#5374=CARTESIAN_POINT('Ctrl Pts',(2.99609686518216,0.154588504271054,1.59896488632222));
#5375=CARTESIAN_POINT('Ctrl Pts',(2.99347740802958,0.198964922639276,1.554588467954));
#5376=CARTESIAN_POINT('Ctrl Pts',(2.99208145165098,0.218202539734559,1.52648632671114));
#5377=CARTESIAN_POINT('Ctrl Pts',(2.99011104995181,0.24372047740942,1.46489582039931));
#5378=CARTESIAN_POINT('Ctrl Pts',(2.98956518577535,0.25,1.43140621366814));
#5379=CARTESIAN_POINT('Ctrl Pts',(2.98956518577535,0.25,1.4));
#5380=CARTESIAN_POINT('Origin',(-1.23743686707646,-1.23743686707646,2.9));
#5381=CARTESIAN_POINT('',(-1.40243686707646,-1.23743686707646,2.9));
#5382=CARTESIAN_POINT('Origin',(-1.23743686707646,-1.23743686707646,2.9));
#5383=CARTESIAN_POINT('',(-1.40243686707646,-1.23743686707646,3.6));
#5384=CARTESIAN_POINT('',(-1.40243686707646,-1.23743686707646,2.9));
#5385=CARTESIAN_POINT('Origin',(-1.23743686707646,-1.23743686707646,3.6));
#5386=CARTESIAN_POINT('Origin',(-1.23743686707646,-1.23743686707646,2.9));
#5387=CARTESIAN_POINT('Origin',(-1.23743686707646,1.23743686707646,2.9));
#5388=CARTESIAN_POINT('',(-1.40243686707646,1.23743686707646,2.9));
#5389=CARTESIAN_POINT('Origin',(-1.23743686707646,1.23743686707646,2.9));
#5390=CARTESIAN_POINT('',(-1.40243686707646,1.23743686707646,3.6));
#5391=CARTESIAN_POINT('',(-1.40243686707646,1.23743686707646,2.9));
#5392=CARTESIAN_POINT('Origin',(-1.23743686707646,1.23743686707646,3.6));
#5393=CARTESIAN_POINT('Origin',(-1.23743686707646,1.23743686707646,2.9));
#5394=CARTESIAN_POINT('Origin',(1.23743686707646,1.23743686707646,2.9));
#5395=CARTESIAN_POINT('',(1.07243686707646,1.23743686707646,2.9));
#5396=CARTESIAN_POINT('Origin',(1.23743686707646,1.23743686707646,2.9));
#5397=CARTESIAN_POINT('',(1.07243686707646,1.23743686707646,3.6));
#5398=CARTESIAN_POINT('',(1.07243686707646,1.23743686707646,2.9));
#5399=CARTESIAN_POINT('Origin',(1.23743686707646,1.23743686707646,3.6));
#5400=CARTESIAN_POINT('Origin',(1.23743686707646,1.23743686707646,2.9));
#5401=CARTESIAN_POINT('Origin',(1.23743686707646,-1.23743686707646,2.9));
#5402=CARTESIAN_POINT('',(1.07243686707646,-1.23743686707646,2.9));
#5403=CARTESIAN_POINT('Origin',(1.23743686707646,-1.23743686707646,2.9));
#5404=CARTESIAN_POINT('',(1.07243686707646,-1.23743686707646,3.6));
#5405=CARTESIAN_POINT('',(1.07243686707646,-1.23743686707646,2.9));
#5406=CARTESIAN_POINT('Origin',(1.23743686707646,-1.23743686707646,3.6));
#5407=CARTESIAN_POINT('Origin',(1.23743686707646,-1.23743686707646,2.9));
#5408=CARTESIAN_POINT('Origin',(-1.76776695296637,-1.76776695296637,2.4));
#5409=CARTESIAN_POINT('',(-1.8139637388702,-1.24480341984751,2.4));
#5410=CARTESIAN_POINT('',(-1.24480341984751,-1.81396373887019,2.4));
#5411=CARTESIAN_POINT('Origin',(0.,0.,2.4));
#5412=CARTESIAN_POINT('Origin',(-1.76776695296637,-1.76776695296637,2.4));
#5413=CARTESIAN_POINT('Origin',(-1.76776695296637,-1.76776695296637,1.8));
#5414=CARTESIAN_POINT('',(-1.8139637388702,-1.24480341984751,1.8));
#5415=CARTESIAN_POINT('',(-1.8139637388702,-1.24480341984751,1.8));
#5416=CARTESIAN_POINT('',(-1.24480341984751,-1.81396373887019,1.8));
#5417=CARTESIAN_POINT('Origin',(-1.76776695296637,-1.76776695296637,1.8));
#5418=CARTESIAN_POINT('',(-1.24480341984751,-1.81396373887019,1.8));
#5419=CARTESIAN_POINT('Origin',(-1.76776695296637,1.76776695296637,1.8));
#5420=CARTESIAN_POINT('',(-1.81396373887019,1.24480341984751,2.4));
#5421=CARTESIAN_POINT('',(-1.81396373887019,1.24480341984751,1.8));
#5422=CARTESIAN_POINT('',(-1.81396373887019,1.24480341984751,1.8));
#5423=CARTESIAN_POINT('',(-1.24480341984751,1.81396373887019,2.4));
#5424=CARTESIAN_POINT('Origin',(-1.76776695296637,1.76776695296637,2.4));
#5425=CARTESIAN_POINT('',(-1.24480341984751,1.81396373887019,1.8));
#5426=CARTESIAN_POINT('',(-1.24480341984751,1.81396373887019,1.8));
#5427=CARTESIAN_POINT('Origin',(-1.76776695296637,1.76776695296637,1.8));
#5428=CARTESIAN_POINT('Origin',(-1.76776695296637,1.76776695296637,2.4));
#5429=CARTESIAN_POINT('Origin',(0.,0.,2.4));
#5430=CARTESIAN_POINT('Origin',(1.76776695296637,1.76776695296637,1.8));
#5431=CARTESIAN_POINT('',(1.24480341984751,1.81396373887019,2.4));
#5432=CARTESIAN_POINT('',(1.24480341984751,1.81396373887019,1.8));
#5433=CARTESIAN_POINT('',(1.24480341984751,1.81396373887019,1.8));
#5434=CARTESIAN_POINT('',(1.81396373887019,1.24480341984751,2.4));
#5435=CARTESIAN_POINT('Origin',(1.76776695296637,1.76776695296637,2.4));
#5436=CARTESIAN_POINT('',(1.81396373887019,1.24480341984751,1.8));
#5437=CARTESIAN_POINT('',(1.81396373887019,1.24480341984751,1.8));
#5438=CARTESIAN_POINT('Origin',(1.76776695296637,1.76776695296637,1.8));
#5439=CARTESIAN_POINT('Origin',(1.76776695296637,1.76776695296637,2.4));
#5440=CARTESIAN_POINT('Origin',(0.,0.,2.4));
#5441=CARTESIAN_POINT('Origin',(1.76776695296637,-1.76776695296637,1.8));
#5442=CARTESIAN_POINT('',(1.81396373887019,-1.24480341984751,2.4));
#5443=CARTESIAN_POINT('',(1.81396373887019,-1.24480341984751,1.8));
#5444=CARTESIAN_POINT('',(1.81396373887019,-1.24480341984751,1.8));
#5445=CARTESIAN_POINT('',(1.24480341984751,-1.8139637388702,2.4));
#5446=CARTESIAN_POINT('Origin',(1.76776695296637,-1.76776695296637,2.4));
#5447=CARTESIAN_POINT('',(1.24480341984751,-1.8139637388702,1.8));
#5448=CARTESIAN_POINT('',(1.24480341984751,-1.8139637388702,1.8));
#5449=CARTESIAN_POINT('Origin',(1.76776695296637,-1.76776695296637,1.8));
#5450=CARTESIAN_POINT('Origin',(1.76776695296637,-1.76776695296637,2.4));
#5451=CARTESIAN_POINT('Origin',(0.,0.,2.4));
#5452=CARTESIAN_POINT('Origin',(0.,0.,1.));
#5453=CARTESIAN_POINT('',(-2.2,-2.69422295812418E-16,3.6));
#5454=CARTESIAN_POINT('Origin',(0.,0.,3.6));
#5455=CARTESIAN_POINT('',(-2.2,-2.69422295812418E-16,1.8));
#5456=CARTESIAN_POINT('',(-2.2,-2.69422295812418E-16,1.));
#5457=CARTESIAN_POINT('Origin',(0.,0.,1.8));
#5458=CARTESIAN_POINT('Origin',(0.,0.,1.8));
#5459=CARTESIAN_POINT('Origin',(0.,0.,1.8));
#5460=CARTESIAN_POINT('Origin',(0.,0.,1.8));
#5461=CARTESIAN_POINT('Origin',(0.,0.,1.8));
#5462=CARTESIAN_POINT('Origin',(0.,0.,1.8));
#5463=CARTESIAN_POINT('',(-3.,-3.67394039744206E-16,1.8));
#5464=CARTESIAN_POINT('Origin',(0.,0.,1.8));
#5465=CARTESIAN_POINT('',(-2.04276695296637,-1.76776695296637,1.8));
#5466=CARTESIAN_POINT('Origin',(-1.76776695296637,-1.76776695296637,1.8));
#5467=CARTESIAN_POINT('',(1.49276695296637,1.76776695296637,1.8));
#5468=CARTESIAN_POINT('Origin',(1.76776695296637,1.76776695296637,1.8));
#5469=CARTESIAN_POINT('',(1.49276695296637,-1.76776695296637,1.8));
#5470=CARTESIAN_POINT('Origin',(1.76776695296637,-1.76776695296637,1.8));
#5471=CARTESIAN_POINT('',(-2.04276695296637,1.76776695296637,1.8));
#5472=CARTESIAN_POINT('Origin',(-1.76776695296637,1.76776695296637,1.8));
#5473=CARTESIAN_POINT('Origin',(-1.76776695296637,-1.76776695296637,0.9));
#5474=CARTESIAN_POINT('',(-2.04276695296637,-1.76776695296637,1.));
#5475=CARTESIAN_POINT('Origin',(-1.76776695296637,-1.76776695296637,1.));
#5476=CARTESIAN_POINT('',(-2.04276695296637,-1.76776695296637,0.9));
#5477=CARTESIAN_POINT('Origin',(-1.76776695296637,1.76776695296637,0.9));
#5478=CARTESIAN_POINT('',(-2.04276695296637,1.76776695296637,1.));
#5479=CARTESIAN_POINT('Origin',(-1.76776695296637,1.76776695296637,1.));
#5480=CARTESIAN_POINT('',(-2.04276695296637,1.76776695296637,0.9));
#5481=CARTESIAN_POINT('Origin',(1.76776695296637,1.76776695296637,0.9));
#5482=CARTESIAN_POINT('',(1.49276695296637,1.76776695296637,1.));
#5483=CARTESIAN_POINT('Origin',(1.76776695296637,1.76776695296637,1.));
#5484=CARTESIAN_POINT('',(1.49276695296637,1.76776695296637,0.9));
#5485=CARTESIAN_POINT('Origin',(1.76776695296637,-1.76776695296637,0.9));
#5486=CARTESIAN_POINT('',(1.49276695296637,-1.76776695296637,1.));
#5487=CARTESIAN_POINT('Origin',(1.76776695296637,-1.76776695296637,1.));
#5488=CARTESIAN_POINT('',(1.49276695296637,-1.76776695296637,0.9));
#5489=CARTESIAN_POINT('Origin',(0.,0.,2.05));
#5490=CARTESIAN_POINT('',(-1.5,-1.83697019872103E-16,2.05));
#5491=CARTESIAN_POINT('Origin',(0.,0.,2.05));
#5492=CARTESIAN_POINT('',(-1.5,1.83697019872103E-16,3.6));
#5493=CARTESIAN_POINT('',(-1.5,-1.83697019872103E-16,2.05));
#5494=CARTESIAN_POINT('Origin',(0.,0.,3.6));
#5495=CARTESIAN_POINT('Origin',(0.,0.,2.05));
#5496=CARTESIAN_POINT('',(-1.02,-1.2491397351303E-16,2.05));
#5497=CARTESIAN_POINT('Origin',(0.,0.,2.05));
#5498=CARTESIAN_POINT('Origin',(0.,0.,1.));
#5499=CARTESIAN_POINT('',(-3.,-3.67394039744206E-16,1.));
#5500=CARTESIAN_POINT('',(-3.,-3.67394039744206E-16,1.));
#5501=CARTESIAN_POINT('Origin',(0.,0.,1.));
#5502=CARTESIAN_POINT('Origin',(0.,0.,1.));
#5503=CARTESIAN_POINT('',(-1.02,-1.2491397351303E-16,1.));
#5504=CARTESIAN_POINT('',(-1.02,-1.2491397351303E-16,1.));
#5505=CARTESIAN_POINT('Origin',(0.,0.,1.));
#5506=CARTESIAN_POINT('Origin',(0.,0.,3.6));
#5507=CARTESIAN_POINT('Origin',(0.,0.,1.));
#5508=CARTESIAN_POINT('',(0.,0.,0.));
#5509=CARTESIAN_POINT('Origin',(0.115470053837925,-0.5,-0.2));
#5510=CARTESIAN_POINT('',(0.23094010767585,-0.5,0.));
#5511=CARTESIAN_POINT('',(0.115470053837925,-0.5,-0.2));
#5512=CARTESIAN_POINT('',(0.23094010767585,-0.5,0.));
#5513=CARTESIAN_POINT('',(0.115470053837925,-0.8,-0.2));
#5514=CARTESIAN_POINT('',(0.115470053837925,-0.5,-0.2));
#5515=CARTESIAN_POINT('',(0.23094010767585,-0.8,0.));
#5516=CARTESIAN_POINT('',(0.23094010767585,-0.8,0.));
#5517=CARTESIAN_POINT('',(0.23094010767585,-0.5,0.));
#5518=CARTESIAN_POINT('Origin',(-0.115470053837925,-0.5,-0.2));
#5519=CARTESIAN_POINT('',(-0.115470053837925,-0.5,-0.2));
#5520=CARTESIAN_POINT('',(0.115470053837925,-0.5,-0.2));
#5521=CARTESIAN_POINT('',(-0.115470053837925,-0.8,-0.2));
#5522=CARTESIAN_POINT('',(-0.115470053837925,-0.5,-0.2));
#5523=CARTESIAN_POINT('',(0.115470053837925,-0.8,-0.2));
#5524=CARTESIAN_POINT('Origin',(-0.23094010767585,-0.5,-2.77555756156289E-17));
#5525=CARTESIAN_POINT('',(-0.23094010767585,-0.5,-2.82820063659975E-17));
#5526=CARTESIAN_POINT('',(-0.115470053837925,-0.5,-0.2));
#5527=CARTESIAN_POINT('',(-0.23094010767585,-0.8,-2.77555756156289E-17));
#5528=CARTESIAN_POINT('',(-0.23094010767585,-0.5,-2.82820063659975E-17));
#5529=CARTESIAN_POINT('',(-0.115470053837925,-0.8,-0.2));
#5530=CARTESIAN_POINT('Origin',(-0.115470053837925,-0.5,0.2));
#5531=CARTESIAN_POINT('',(-0.115470053837925,-0.5,0.2));
#5532=CARTESIAN_POINT('',(-0.23094010767585,-0.5,-2.82820063659975E-17));
#5533=CARTESIAN_POINT('',(-0.115470053837925,-0.8,0.2));
#5534=CARTESIAN_POINT('',(-0.115470053837925,-0.5,0.2));
#5535=CARTESIAN_POINT('',(-0.23094010767585,-0.8,-2.82820063659975E-17));
#5536=CARTESIAN_POINT('Origin',(0.115470053837925,-0.5,0.2));
#5537=CARTESIAN_POINT('',(0.115470053837925,-0.5,0.2));
#5538=CARTESIAN_POINT('',(-0.115470053837925,-0.5,0.2));
#5539=CARTESIAN_POINT('',(0.115470053837925,-0.8,0.2));
#5540=CARTESIAN_POINT('',(0.115470053837925,-0.5,0.2));
#5541=CARTESIAN_POINT('',(-0.115470053837925,-0.8,0.2));
#5542=CARTESIAN_POINT('Origin',(0.23094010767585,-0.5,0.));
#5543=CARTESIAN_POINT('',(0.115470053837925,-0.5,0.2));
#5544=CARTESIAN_POINT('',(0.115470053837925,-0.8,0.2));
#5545=CARTESIAN_POINT('Origin',(0.,-0.5,0.));
#5546=CARTESIAN_POINT('Origin',(0.,-0.8,0.));
#5547=CARTESIAN_POINT('Origin',(0.,-1.4,0.));
#5548=CARTESIAN_POINT('',(-0.24505,-1.4,3.00099698131059E-17));
#5549=CARTESIAN_POINT('Origin',(0.,-1.4,0.));
#5550=CARTESIAN_POINT('Origin',(0.375,0.5,0.));
#5551=CARTESIAN_POINT('',(-0.375,0.5,-4.59242549680257E-17));
#5552=CARTESIAN_POINT('Origin',(0.,0.5,0.));
#5553=CARTESIAN_POINT('Origin',(0.,0.475,0.));
#5554=CARTESIAN_POINT('',(-0.425,0.45,-5.20474889637625E-17));
#5555=CARTESIAN_POINT('Origin',(0.,0.45,0.));
#5556=CARTESIAN_POINT('',(-0.4,0.475,-4.89858719658941E-17));
#5557=CARTESIAN_POINT('Origin',(0.,0.24,0.));
#5558=CARTESIAN_POINT('',(-0.425,0.0299999999999998,-5.20474889637625E-17));
#5559=CARTESIAN_POINT('Origin',(0.,0.0299999999999998,0.));
#5560=CARTESIAN_POINT('',(-0.425,0.24,-5.20474889637625E-17));
#5561=CARTESIAN_POINT('Origin',(0.,0.0150000000000001,0.));
#5562=CARTESIAN_POINT('',(-0.395,4.85722573273506E-17,-4.83735485663204E-17));
#5563=CARTESIAN_POINT('Origin',(0.,0.,0.));
#5564=CARTESIAN_POINT('',(-0.41,0.0150000000000001,-5.02105187650415E-17));
#5565=CARTESIAN_POINT('Origin',(0.27,0.,0.));
#5566=CARTESIAN_POINT('',(-0.27,0.,-3.30654635769785E-17));
#5567=CARTESIAN_POINT('Origin',(0.,0.,0.));
#5568=CARTESIAN_POINT('Origin',(0.,-0.02,0.));
#5569=CARTESIAN_POINT('',(-0.24505,-0.0498999999999999,3.00099698131059E-17));
#5570=CARTESIAN_POINT('Origin',(0.,-0.0498999999999999,0.));
#5571=CARTESIAN_POINT('',(-0.26,-0.02,-3.18408167778312E-17));
#5572=CARTESIAN_POINT('Origin',(0.,-0.995,0.));
#5573=CARTESIAN_POINT('',(-0.24505,-0.995,-3.00099698131059E-17));
#5574=CARTESIAN_POINT('',(0.,0.,0.));
#5575=CARTESIAN_POINT('',(0.,0.,0.));
#5576=CARTESIAN_POINT('',(0.,0.,0.));
#5577=CARTESIAN_POINT('Origin',(0.762563132923542,2.2266647480613,5.65));
#5578=CARTESIAN_POINT('',(0.597563132923542,2.2266647480613,5.65));
#5579=CARTESIAN_POINT('Origin',(0.762563132923542,2.2266647480613,5.65));
#5580=CARTESIAN_POINT('',(0.597563132923542,2.2266647480613,6.35));
#5581=CARTESIAN_POINT('',(0.597563132923542,2.2266647480613,5.65));
#5582=CARTESIAN_POINT('Origin',(0.762563132923542,2.2266647480613,6.35));
#5583=CARTESIAN_POINT('Origin',(0.762563132923542,2.2266647480613,5.65));
#5584=CARTESIAN_POINT('Origin',(0.762563132923542,4.70153848221421,5.65));
#5585=CARTESIAN_POINT('',(0.597563132923542,4.70153848221421,5.65));
#5586=CARTESIAN_POINT('Origin',(0.762563132923542,4.70153848221421,5.65));
#5587=CARTESIAN_POINT('',(0.597563132923542,4.70153848221421,6.35));
#5588=CARTESIAN_POINT('',(0.597563132923542,4.70153848221421,5.65));
#5589=CARTESIAN_POINT('Origin',(0.762563132923542,4.70153848221421,6.35));
#5590=CARTESIAN_POINT('Origin',(0.762563132923542,4.70153848221421,5.65));
#5591=CARTESIAN_POINT('Origin',(3.23743686707646,4.70153848221421,5.65));
#5592=CARTESIAN_POINT('',(3.07243686707646,4.70153848221421,5.65));
#5593=CARTESIAN_POINT('Origin',(3.23743686707646,4.70153848221421,5.65));
#5594=CARTESIAN_POINT('',(3.07243686707646,4.70153848221421,6.35));
#5595=CARTESIAN_POINT('',(3.07243686707646,4.70153848221421,5.65));
#5596=CARTESIAN_POINT('Origin',(3.23743686707646,4.70153848221421,6.35));
#5597=CARTESIAN_POINT('Origin',(3.23743686707646,4.70153848221421,5.65));
#5598=CARTESIAN_POINT('Origin',(3.23743686707646,2.2266647480613,5.65));
#5599=CARTESIAN_POINT('',(3.07243686707646,2.2266647480613,5.65));
#5600=CARTESIAN_POINT('Origin',(3.23743686707646,2.2266647480613,5.65));
#5601=CARTESIAN_POINT('',(3.07243686707646,2.2266647480613,6.35));
#5602=CARTESIAN_POINT('',(3.07243686707646,2.2266647480613,5.65));
#5603=CARTESIAN_POINT('Origin',(3.23743686707646,2.2266647480613,6.35));
#5604=CARTESIAN_POINT('Origin',(3.23743686707646,2.2266647480613,5.65));
#5605=CARTESIAN_POINT('Origin',(2.,3.46410161513775,4.8));
#5606=CARTESIAN_POINT('',(0.5,3.46410161513775,4.8));
#5607=CARTESIAN_POINT('Origin',(2.,3.46410161513775,4.8));
#5608=CARTESIAN_POINT('',(0.5,3.46410161513775,6.35));
#5609=CARTESIAN_POINT('',(0.5,3.46410161513775,4.8));
#5610=CARTESIAN_POINT('Origin',(2.,3.46410161513775,6.35));
#5611=CARTESIAN_POINT('Origin',(2.,3.46410161513775,4.8));
#5612=CARTESIAN_POINT('',(0.98,3.46410161513775,4.8));
#5613=CARTESIAN_POINT('Origin',(2.,3.46410161513775,4.8));
#5614=CARTESIAN_POINT('Origin',(2.,3.46410161513775,4.5));
#5615=CARTESIAN_POINT('',(0.98,3.46410161513775,4.6));
#5616=CARTESIAN_POINT('Origin',(2.,3.46410161513775,4.6));
#5617=CARTESIAN_POINT('',(0.98,3.46410161513775,4.5));
#5618=CARTESIAN_POINT('Origin',(2.,3.46410161513775,4.6));
#5619=CARTESIAN_POINT('',(-0.2,3.46410161513775,6.35));
#5620=CARTESIAN_POINT('Origin',(2.,3.46410161513775,6.35));
#5621=CARTESIAN_POINT('',(-0.2,3.46410161513775,4.6));
#5622=CARTESIAN_POINT('',(-0.2,3.46410161513775,4.6));
#5623=CARTESIAN_POINT('Origin',(2.,3.46410161513775,4.6));
#5624=CARTESIAN_POINT('',(0.422084233303501,1.93107133715542,5.6));
#5625=CARTESIAN_POINT('',(0.422084233303501,1.93107133715542,4.8));
#5626=CARTESIAN_POINT('',(0.4220842333035,1.93107133715542,4.6));
#5627=CARTESIAN_POINT('',(1.46131471784483,1.33107133715542,5.6));
#5628=CARTESIAN_POINT('Origin',(2.,3.46410161513775,5.6));
#5629=CARTESIAN_POINT('',(1.46131471784483,1.33107133715542,4.8));
#5630=CARTESIAN_POINT('',(1.46131471784483,1.33107133715542,4.6));
#5631=CARTESIAN_POINT('Origin',(2.,3.46410161513775,4.8));
#5632=CARTESIAN_POINT('Origin',(2.,3.46410161513775,6.35));
#5633=CARTESIAN_POINT('Origin',(2.,3.46410161513775,4.6));
#5634=CARTESIAN_POINT('Origin',(0.519615242270663,-0.3,4.8));
#5635=CARTESIAN_POINT('',(0.919615242270663,0.392820323027551,5.6));
#5636=CARTESIAN_POINT('',(2.51961524227066,3.16410161513775,5.6));
#5637=CARTESIAN_POINT('',(0.919615242270663,0.392820323027551,4.8));
#5638=CARTESIAN_POINT('',(0.919615242270663,0.392820323027551,4.8));
#5639=CARTESIAN_POINT('',(2.51961524227066,3.16410161513775,4.8));
#5640=CARTESIAN_POINT('Origin',(0.,0.,5.6));
#5641=CARTESIAN_POINT('',(-0.119615242270663,0.992820323027551,5.6));
#5642=CARTESIAN_POINT('',(-0.519615242270663,0.3,5.6));
#5643=CARTESIAN_POINT('Origin',(0.,0.,5.6));
#5644=CARTESIAN_POINT('Origin',(1.48038475772934,3.76410161513775,4.8));
#5645=CARTESIAN_POINT('',(-0.119615242270663,0.992820323027551,4.8));
#5646=CARTESIAN_POINT('',(-0.519615242270663,0.3,4.8));
#5647=CARTESIAN_POINT('',(-0.119615242270663,0.992820323027551,4.8));
#5648=CARTESIAN_POINT('Origin',(0.,0.,4.8));
#5649=CARTESIAN_POINT('Origin',(0.,0.,4.8));
#5650=CARTESIAN_POINT('Origin',(0.,0.,4.8));
#5651=CARTESIAN_POINT('',(-0.7,-8.57252759403147E-17,4.8));
#5652=CARTESIAN_POINT('Origin',(0.,0.,4.8));
#5653=CARTESIAN_POINT('Origin',(0.,0.,2.95));
#5654=CARTESIAN_POINT('',(-0.7,-8.57252759403147E-17,2.95));
#5655=CARTESIAN_POINT('Origin',(0.,0.,2.95));
#5656=CARTESIAN_POINT('',(-0.5,6.12323399573677E-17,2.95));
#5657=CARTESIAN_POINT('Origin',(0.,0.,2.95));
#5658=CARTESIAN_POINT('Origin',(0.,0.,2.95));
#5659=CARTESIAN_POINT('',(-0.7,-8.57252759403147E-17,2.95));
#5660=CARTESIAN_POINT('Origin',(0.,0.,1.));
#5661=CARTESIAN_POINT('',(-0.5,-6.12323399573677E-17,1.));
#5662=CARTESIAN_POINT('',(-0.5,-6.12323399573677E-17,1.));
#5663=CARTESIAN_POINT('Origin',(0.,0.,1.));
#5664=CARTESIAN_POINT('Origin',(0.,0.,1.));
#5665=CARTESIAN_POINT('',(0.,0.,0.));
#5666=CARTESIAN_POINT('',(0.,0.,0.));
#5667=CARTESIAN_POINT('Origin',(0.,0.,0.));
#5668=CARTESIAN_POINT('',(-0.976185,-0.246528389340863,-1.19548183562566E-16));
#5669=CARTESIAN_POINT('',(-1.19548183562566E-16,-0.246528389340863,0.976185));
#5670=CARTESIAN_POINT('Origin',(0.,-0.246528389340863,0.));
#5671=CARTESIAN_POINT('Origin',(0.,-0.246528389340863,0.));
#5672=CARTESIAN_POINT('',(-1.19548183562566E-16,0.246528389340863,0.976185));
#5673=CARTESIAN_POINT('Origin',(-1.22464679914735E-16,0.,1.));
#5674=CARTESIAN_POINT('',(-0.976185,0.246528389340863,1.19548183562566E-16));
#5675=CARTESIAN_POINT('Origin',(0.,0.246528389340863,0.));
#5676=CARTESIAN_POINT('Origin',(0.,0.246528389340863,0.));
#5677=CARTESIAN_POINT('Origin',(0.,0.,0.));
#5678=CARTESIAN_POINT('',(-0.976185,0.45,-1.19548183562566E-16));
#5679=CARTESIAN_POINT('',(-0.976185,0.,-1.19548183562566E-16));
#5680=CARTESIAN_POINT('Origin',(0.,0.45,0.));
#5681=CARTESIAN_POINT('Origin',(0.,0.,0.));
#5682=CARTESIAN_POINT('',(-0.5,-0.39,-6.12323399573677E-17));
#5683=CARTESIAN_POINT('Origin',(0.,-0.39,0.));
#5684=CARTESIAN_POINT('',(-0.5,0.39,-6.12323399573677E-17));
#5685=CARTESIAN_POINT('',(-0.5,0.,-6.12323399573677E-17));
#5686=CARTESIAN_POINT('Origin',(0.,0.39,0.));
#5687=CARTESIAN_POINT('Origin',(0.,0.42,0.));
#5688=CARTESIAN_POINT('',(-0.56,0.45,-6.85802207522518E-17));
#5689=CARTESIAN_POINT('',(-0.53,0.42,-6.49062803548097E-17));
#5690=CARTESIAN_POINT('Origin',(0.,0.45,0.));
#5691=CARTESIAN_POINT('Origin',(0.976185,0.45,0.));
#5692=CARTESIAN_POINT('Origin',(0.,0.,0.));
#5693=CARTESIAN_POINT('',(-0.976185,-0.45,-1.19548183562566E-16));
#5694=CARTESIAN_POINT('Origin',(0.,-0.45,0.));
#5695=CARTESIAN_POINT('',(-0.976185,0.,-1.19548183562566E-16));
#5696=CARTESIAN_POINT('Origin',(0.56,-0.45,0.));
#5697=CARTESIAN_POINT('',(-0.56,-0.45,-6.85802207522518E-17));
#5698=CARTESIAN_POINT('Origin',(0.,-0.45,0.));
#5699=CARTESIAN_POINT('Origin',(0.,-0.42,0.));
#5700=CARTESIAN_POINT('',(-0.53,-0.42,-6.49062803548097E-17));
#5701=CARTESIAN_POINT('',(0.,0.,0.));
#5702=CARTESIAN_POINT('Origin',(0.,0.,0.));
#5703=CARTESIAN_POINT('',(-1.023815,0.246528389340863,-1.25381176266905E-16));
#5704=CARTESIAN_POINT('',(-1.25381176266905E-16,0.246528389340863,1.023815));
#5705=CARTESIAN_POINT('Origin',(0.,0.246528389340863,0.));
#5706=CARTESIAN_POINT('Origin',(0.,0.246528389340863,0.));
#5707=CARTESIAN_POINT('',(-1.25381176266905E-16,-0.246528389340863,1.023815));
#5708=CARTESIAN_POINT('Origin',(-1.22464679914735E-16,0.,1.));
#5709=CARTESIAN_POINT('',(-1.023815,-0.246528389340863,1.25381176266905E-16));
#5710=CARTESIAN_POINT('Origin',(0.,-0.246528389340863,0.));
#5711=CARTESIAN_POINT('Origin',(0.,-0.246528389340863,0.));
#5712=CARTESIAN_POINT('Origin',(0.,0.,0.));
#5713=CARTESIAN_POINT('',(-1.023815,-0.45,-1.25381176266905E-16));
#5714=CARTESIAN_POINT('Origin',(0.,-0.45,0.));
#5715=CARTESIAN_POINT('',(-1.023815,0.,-1.25381176266905E-16));
#5716=CARTESIAN_POINT('Origin',(1.44,0.45,0.));
#5717=CARTESIAN_POINT('',(-1.44,0.45,-1.76349139077219E-16));
#5718=CARTESIAN_POINT('Origin',(0.,0.45,0.));
#5719=CARTESIAN_POINT('',(-1.023815,0.45,-1.25381176266905E-16));
#5720=CARTESIAN_POINT('Origin',(0.,0.45,0.));
#5721=CARTESIAN_POINT('Origin',(0.,0.42,0.));
#5722=CARTESIAN_POINT('',(-1.5,0.39,-1.83697019872103E-16));
#5723=CARTESIAN_POINT('Origin',(0.,0.39,0.));
#5724=CARTESIAN_POINT('',(-1.47,0.42,-1.80023079474661E-16));
#5725=CARTESIAN_POINT('Origin',(0.,0.,0.));
#5726=CARTESIAN_POINT('',(-1.5,-0.39,-1.83697019872103E-16));
#5727=CARTESIAN_POINT('Origin',(0.,-0.39,0.));
#5728=CARTESIAN_POINT('',(-1.5,0.,-1.83697019872103E-16));
#5729=CARTESIAN_POINT('Origin',(0.,-0.42,0.));
#5730=CARTESIAN_POINT('',(-1.44,-0.45,-1.76349139077219E-16));
#5731=CARTESIAN_POINT('Origin',(0.,-0.45,0.));
#5732=CARTESIAN_POINT('',(-1.47,-0.42,-1.80023079474661E-16));
#5733=CARTESIAN_POINT('Origin',(1.023815,-0.45,0.));
#5734=CARTESIAN_POINT('Origin',(0.,0.,0.));
#5735=CARTESIAN_POINT('',(-1.023815,0.,-1.25381176266905E-16));
#5736=CARTESIAN_POINT('',(0.,0.,0.));
#5737=CARTESIAN_POINT('Origin',(1.,0.,0.));
#5738=CARTESIAN_POINT('',(1.,-1.78583896120461E-33,0.23815));
#5739=CARTESIAN_POINT('',(1.,-1.78583896120461E-33,-0.23815));
#5740=CARTESIAN_POINT('Origin',(1.,0.,0.));
#5741=CARTESIAN_POINT('Origin',(0.707106781186548,0.,-0.707106781186547));
#5742=CARTESIAN_POINT('',(0.875504261126124,-1.78583896120461E-33,-0.538709301246971));
#5743=CARTESIAN_POINT('',(0.538709301246971,-1.78583896120461E-33,-0.875504261126124));
#5744=CARTESIAN_POINT('Origin',(0.707106781186548,0.,-0.707106781186547));
#5745=CARTESIAN_POINT('Origin',(6.12323399573677E-17,0.,-1.));
#5746=CARTESIAN_POINT('',(0.23815,-1.78583896120461E-33,-1.));
#5747=CARTESIAN_POINT('',(-0.23815,-1.78583896120461E-33,-1.));
#5748=CARTESIAN_POINT('Origin',(6.12323399573677E-17,0.,-1.));
#5749=CARTESIAN_POINT('Origin',(-0.707106781186547,0.,-0.707106781186548));
#5750=CARTESIAN_POINT('',(-0.538709301246971,-1.78583896120461E-33,-0.875504261126124));
#5751=CARTESIAN_POINT('',(-0.875504261126124,-1.78583896120461E-33,-0.538709301246971));
#5752=CARTESIAN_POINT('Origin',(-0.707106781186547,0.,-0.707106781186548));
#5753=CARTESIAN_POINT('Origin',(-1.,0.,-1.22464679914735E-16));
#5754=CARTESIAN_POINT('',(-1.,-1.78583896120461E-33,-0.23815));
#5755=CARTESIAN_POINT('',(-1.,-1.78583896120461E-33,0.23815));
#5756=CARTESIAN_POINT('Origin',(-1.,0.,-1.22464679914735E-16));
#5757=CARTESIAN_POINT('Origin',(-0.707106781186548,0.,0.707106781186547));
#5758=CARTESIAN_POINT('',(-0.875504261126124,-7.94881478324376E-33,0.538709301246971));
#5759=CARTESIAN_POINT('',(-0.538709301246971,4.37713686083455E-33,0.875504261126124));
#5760=CARTESIAN_POINT('Origin',(-0.707106781186548,0.,0.707106781186547));
#5761=CARTESIAN_POINT('Origin',(-1.83697019872103E-16,0.,1.));
#5762=CARTESIAN_POINT('',(-0.23815,-1.78583896120461E-33,1.));
#5763=CARTESIAN_POINT('',(0.23815,-1.78583896120461E-33,1.));
#5764=CARTESIAN_POINT('Origin',(-1.83697019872103E-16,0.,1.));
#5765=CARTESIAN_POINT('Origin',(0.707106781186547,0.,0.707106781186548));
#5766=CARTESIAN_POINT('',(0.538709301246971,-4.86732687222419E-33,0.875504261126124));
#5767=CARTESIAN_POINT('',(0.875504261126124,1.29564894981497E-33,0.538709301246971));
#5768=CARTESIAN_POINT('Origin',(0.707106781186547,0.,0.707106781186548));
#5769=CARTESIAN_POINT('',(0.,0.,0.));
#5770=CARTESIAN_POINT('Origin',(0.707106781186547,0.,0.707106781186548));
#5771=CARTESIAN_POINT('',(0.504455939115715,-0.04763,0.841298510752802));
#5772=CARTESIAN_POINT('',(0.841298510752802,-0.04763,0.504455939115715));
#5773=CARTESIAN_POINT('Ctrl Pts',(0.504455939115715,-0.04763,0.841298510752802));
#5774=CARTESIAN_POINT('Ctrl Pts',(0.508899795931835,-0.0740444353928835,
0.838633903678357));
#5775=CARTESIAN_POINT('Ctrl Pts',(0.517157748491652,-0.0999305678883309,
0.833661031856294));
#5776=CARTESIAN_POINT('Ctrl Pts',(0.537715343527944,-0.142345102874864,
0.820511285096538));
#5777=CARTESIAN_POINT('Ctrl Pts',(0.548874290046456,-0.159766064500479,
0.813159949759));
#5778=CARTESIAN_POINT('Ctrl Pts',(0.573915184558107,-0.190326085855194,
0.795684265985089));
#5779=CARTESIAN_POINT('Ctrl Pts',(0.587792702767295,-0.203463743702801,
0.78555112003688));
#5780=CARTESIAN_POINT('Ctrl Pts',(0.615966552324775,-0.224161999508995,
0.763642258217233));
#5781=CARTESIAN_POINT('Ctrl Pts',(0.631684198665438,-0.232861760990032,
0.750785745543687));
#5782=CARTESIAN_POINT('Ctrl Pts',(0.663382628119203,-0.244251601209411,
0.722929908501543));
#5783=CARTESIAN_POINT('Ctrl Pts',(0.679352081686668,-0.246942143572133,
0.707917883896095));
#5784=CARTESIAN_POINT('Ctrl Pts',(0.707917883896095,-0.246942143572133,
0.679352081686668));
#5785=CARTESIAN_POINT('Ctrl Pts',(0.722929908501543,-0.244251601209411,
0.663382628119203));
#5786=CARTESIAN_POINT('Ctrl Pts',(0.750785745543687,-0.232861760990032,
0.631684198665439));
#5787=CARTESIAN_POINT('Ctrl Pts',(0.763642258217232,-0.224161999508995,
0.615966552324775));
#5788=CARTESIAN_POINT('Ctrl Pts',(0.78555112003688,-0.203463743702801,0.587792702767295));
#5789=CARTESIAN_POINT('Ctrl Pts',(0.795684265985088,-0.190326085855194,
0.573915184558108));
#5790=CARTESIAN_POINT('Ctrl Pts',(0.813159949759,-0.15976606450048,0.548874290046456));
#5791=CARTESIAN_POINT('Ctrl Pts',(0.820511285096538,-0.142345102874864,
0.537715343527944));
#5792=CARTESIAN_POINT('Ctrl Pts',(0.833661031856294,-0.099930567888331,
0.517157748491653));
#5793=CARTESIAN_POINT('Ctrl Pts',(0.838633903678357,-0.0740444353928835,
0.508899795931835));
#5794=CARTESIAN_POINT('Ctrl Pts',(0.841298510752801,-0.0476299999999999,
0.504455939115715));
#5795=CARTESIAN_POINT('',(0.528110872004958,-0.04763,0.871530771444223));
#5796=CARTESIAN_POINT('Origin',(0.707106781186547,-0.04763,0.707106781186548));
#5797=CARTESIAN_POINT('',(0.871530771444223,-0.04763,0.528110872004959));
#5798=CARTESIAN_POINT('Ctrl Pts',(0.871530771444223,-0.0476300000000001,
0.528110872004958));
#5799=CARTESIAN_POINT('Ctrl Pts',(0.87014664509073,-0.0609922781173483,
0.530395067942936));
#5800=CARTESIAN_POINT('Ctrl Pts',(0.868149331745851,-0.0742967091364493,
0.533674141594226));
#5801=CARTESIAN_POINT('Ctrl Pts',(0.85981294420286,-0.115492077056649,0.54708917182331));
#5802=CARTESIAN_POINT('Ctrl Pts',(0.850993704737257,-0.141695629206859,
0.560922177770136));
#5803=CARTESIAN_POINT('Ctrl Pts',(0.830754510485543,-0.181890537957859,
0.590422647829571));
#5804=CARTESIAN_POINT('Ctrl Pts',(0.816896541396381,-0.201072148666545,
0.609616703125488));
#5805=CARTESIAN_POINT('Ctrl Pts',(0.792310597819928,-0.223955109275652,
0.641117951819998));
#5806=CARTESIAN_POINT('Ctrl Pts',(0.779109323683612,-0.232742381310829,
0.657208095763053));
#5807=CARTESIAN_POINT('Ctrl Pts',(0.750552691816206,-0.244234834628584,
0.68964083160521));
#5808=CARTESIAN_POINT('Ctrl Pts',(0.735185187071673,-0.246942143572133,
0.705971972091755));
#5809=CARTESIAN_POINT('Ctrl Pts',(0.705971972091754,-0.246942143572133,
0.735185187071673));
#5810=CARTESIAN_POINT('Ctrl Pts',(0.689640831605209,-0.244234834628584,
0.750552691816206));
#5811=CARTESIAN_POINT('Ctrl Pts',(0.657208095763052,-0.232742381310829,
0.779109323683612));
#5812=CARTESIAN_POINT('Ctrl Pts',(0.641117951819998,-0.223955109275652,
0.792310597819928));
#5813=CARTESIAN_POINT('Ctrl Pts',(0.609616703125487,-0.201072148666545,
0.816896541396382));
#5814=CARTESIAN_POINT('Ctrl Pts',(0.590422647829571,-0.181890537957858,
0.830754510485544));
#5815=CARTESIAN_POINT('Ctrl Pts',(0.560922177770135,-0.141695629206858,
0.850993704737257));
#5816=CARTESIAN_POINT('Ctrl Pts',(0.547089171823309,-0.115492077056649,
0.859812944202861));
#5817=CARTESIAN_POINT('Ctrl Pts',(0.533674141594226,-0.0742967091364491,
0.868149331745852));
#5818=CARTESIAN_POINT('Ctrl Pts',(0.530395067942936,-0.0609922781173483,
0.870146645090731));
#5819=CARTESIAN_POINT('Ctrl Pts',(0.528110872004958,-0.0476300000000001,
0.871530771444223));
#5820=CARTESIAN_POINT('Origin',(0.707106781186547,-0.04763,0.707106781186548));
#5821=CARTESIAN_POINT('Origin',(0.,-0.166705,0.));
#5822=CARTESIAN_POINT('',(0.242834539687906,-0.04763,0.989696097314));
#5823=CARTESIAN_POINT('Origin',(0.,-0.04763,0.));
#5824=CARTESIAN_POINT('',(-0.242834539687907,-0.04763,0.989696097314));
#5825=CARTESIAN_POINT('Ctrl Pts',(0.242834539687906,-0.04763,0.989696097314));
#5826=CARTESIAN_POINT('Ctrl Pts',(0.24024064412003,-0.0609922781173483,
0.990332542620729));
#5827=CARTESIAN_POINT('Ctrl Pts',(0.236509675094874,-0.0742967091364492,
0.991238884025248));
#5828=CARTESIAN_POINT('Ctrl Pts',(0.221129100087819,-0.115492077056649,
0.994830026707808));
#5829=CARTESIAN_POINT('Ctrl Pts',(0.205111543747588,-0.141695629206859,
0.998375294985966));
#5830=CARTESIAN_POINT('Ctrl Pts',(0.169940289819232,-0.181890537957859,
1.00492400591205));
#5831=CARTESIAN_POINT('Ctrl Pts',(0.1465689792446,-0.201072148666545,1.00869718865384));
#5832=CARTESIAN_POINT('Ctrl Pts',(0.106909345252087,-0.223955109275652,
1.01358704779679));
#5833=CARTESIAN_POINT('Ctrl Pts',(0.0861971848975941,-0.232742381310829,
1.0156297872271));
#5834=CARTESIAN_POINT('Ctrl Pts',(0.0430711894098822,-0.244234834628584,
1.01837060663223));
#5835=CARTESIAN_POINT('Ctrl Pts',(0.0206568624125605,-0.246942143572133,
1.019052));
#5836=CARTESIAN_POINT('Ctrl Pts',(-0.0206568624125608,-0.246942143572133,
1.019052));
#5837=CARTESIAN_POINT('Ctrl Pts',(-0.0430711894098825,-0.244234834628584,
1.01837060663223));
#5838=CARTESIAN_POINT('Ctrl Pts',(-0.0861971848975943,-0.232742381310829,
1.0156297872271));
#5839=CARTESIAN_POINT('Ctrl Pts',(-0.106909345252088,-0.223955109275652,
1.01358704779679));
#5840=CARTESIAN_POINT('Ctrl Pts',(-0.1465689792446,-0.201072148666545,1.00869718865384));
#5841=CARTESIAN_POINT('Ctrl Pts',(-0.169940289819232,-0.181890537957859,
1.00492400591205));
#5842=CARTESIAN_POINT('Ctrl Pts',(-0.205111543747588,-0.141695629206859,
0.998375294985966));
#5843=CARTESIAN_POINT('Ctrl Pts',(-0.221129100087819,-0.115492077056649,
0.994830026707808));
#5844=CARTESIAN_POINT('Ctrl Pts',(-0.236509675094875,-0.0742967091364493,
0.991238884025248));
#5845=CARTESIAN_POINT('Ctrl Pts',(-0.24024064412003,-0.0609922781173483,
0.990332542620729));
#5846=CARTESIAN_POINT('Ctrl Pts',(-0.242834539687907,-0.04763,0.989696097314));
#5847=CARTESIAN_POINT('',(-0.528110872004959,-0.04763,0.871530771444223));
#5848=CARTESIAN_POINT('Origin',(0.,-0.04763,0.));
#5849=CARTESIAN_POINT('',(-0.871530771444223,-0.04763,0.528110872004958));
#5850=CARTESIAN_POINT('Ctrl Pts',(-0.528110872004958,-0.0476300000000001,
0.871530771444223));
#5851=CARTESIAN_POINT('Ctrl Pts',(-0.530395067942936,-0.0609922781173484,
0.87014664509073));
#5852=CARTESIAN_POINT('Ctrl Pts',(-0.533674141594226,-0.0742967091364493,
0.868149331745851));
#5853=CARTESIAN_POINT('Ctrl Pts',(-0.54708917182331,-0.115492077056649,
0.85981294420286));
#5854=CARTESIAN_POINT('Ctrl Pts',(-0.560922177770136,-0.141695629206859,
0.850993704737257));
#5855=CARTESIAN_POINT('Ctrl Pts',(-0.590422647829571,-0.181890537957859,
0.830754510485543));
#5856=CARTESIAN_POINT('Ctrl Pts',(-0.609616703125488,-0.201072148666545,
0.816896541396381));
#5857=CARTESIAN_POINT('Ctrl Pts',(-0.641117951819998,-0.223955109275652,
0.792310597819928));
#5858=CARTESIAN_POINT('Ctrl Pts',(-0.657208095763053,-0.232742381310829,
0.779109323683611));
#5859=CARTESIAN_POINT('Ctrl Pts',(-0.68964083160521,-0.244234834628584,
0.750552691816205));
#5860=CARTESIAN_POINT('Ctrl Pts',(-0.705971972091755,-0.246942143572133,
0.735185187071673));
#5861=CARTESIAN_POINT('Ctrl Pts',(-0.735185187071673,-0.246942143572133,
0.705971972091754));
#5862=CARTESIAN_POINT('Ctrl Pts',(-0.750552691816206,-0.244234834628584,
0.689640831605209));
#5863=CARTESIAN_POINT('Ctrl Pts',(-0.779109323683612,-0.232742381310829,
0.657208095763052));
#5864=CARTESIAN_POINT('Ctrl Pts',(-0.792310597819928,-0.223955109275652,
0.641117951819998));
#5865=CARTESIAN_POINT('Ctrl Pts',(-0.816896541396382,-0.201072148666545,
0.609616703125487));
#5866=CARTESIAN_POINT('Ctrl Pts',(-0.830754510485544,-0.181890537957858,
0.590422647829571));
#5867=CARTESIAN_POINT('Ctrl Pts',(-0.850993704737257,-0.141695629206858,
0.560922177770135));
#5868=CARTESIAN_POINT('Ctrl Pts',(-0.859812944202861,-0.115492077056649,
0.547089171823309));
#5869=CARTESIAN_POINT('Ctrl Pts',(-0.868149331745852,-0.0742967091364491,
0.533674141594226));
#5870=CARTESIAN_POINT('Ctrl Pts',(-0.870146645090731,-0.0609922781173483,
0.530395067942936));
#5871=CARTESIAN_POINT('Ctrl Pts',(-0.871530771444223,-0.04763,0.528110872004958));
#5872=CARTESIAN_POINT('',(-0.989696097314,-0.04763,0.242834539687906));
#5873=CARTESIAN_POINT('Origin',(0.,-0.04763,0.));
#5874=CARTESIAN_POINT('',(-1.019052,-0.246942143572133,1.248489836334E-16));
#5875=CARTESIAN_POINT('Ctrl Pts',(-0.989696097314,-0.04763,0.242834539687906));
#5876=CARTESIAN_POINT('Ctrl Pts',(-0.990332542620729,-0.0609922781173483,
0.24024064412003));
#5877=CARTESIAN_POINT('Ctrl Pts',(-0.991238884025248,-0.0742967091364492,
0.236509675094874));
#5878=CARTESIAN_POINT('Ctrl Pts',(-0.994830026707808,-0.115492077056649,
0.221129100087819));
#5879=CARTESIAN_POINT('Ctrl Pts',(-0.998375294985966,-0.141695629206859,
0.205111543747588));
#5880=CARTESIAN_POINT('Ctrl Pts',(-1.00492400591205,-0.181890537957859,
0.169940289819232));
#5881=CARTESIAN_POINT('Ctrl Pts',(-1.00869718865384,-0.201072148666545,
0.1465689792446));
#5882=CARTESIAN_POINT('Ctrl Pts',(-1.01358704779679,-0.223955109275652,
0.106909345252088));
#5883=CARTESIAN_POINT('Ctrl Pts',(-1.0156297872271,-0.232742381310829,0.0861971848975944));
#5884=CARTESIAN_POINT('Ctrl Pts',(-1.01837060663223,-0.244234834628584,
0.0430711894098825));
#5885=CARTESIAN_POINT('Ctrl Pts',(-1.019052,-0.246942143572133,0.0206568624125608));
#5886=CARTESIAN_POINT('Ctrl Pts',(-1.019052,-0.246942143572133,1.2490009027033E-16));
#5887=CARTESIAN_POINT('',(-1.019052,-0.28578,1.24797876996471E-16));
#5888=CARTESIAN_POINT('',(-1.019052,-0.166705,1.24797876996471E-16));
#5889=CARTESIAN_POINT('Origin',(0.,-0.28578,0.));
#5890=CARTESIAN_POINT('',(-0.989696097314,-0.04763,-0.242834539687906));
#5891=CARTESIAN_POINT('Ctrl Pts',(-1.019052,-0.246942143572133,1.2490009027033E-16));
#5892=CARTESIAN_POINT('Ctrl Pts',(-1.019052,-0.246942143572133,-0.0206568624125605));
#5893=CARTESIAN_POINT('Ctrl Pts',(-1.01837060663223,-0.244234834628584,
-0.0430711894098822));
#5894=CARTESIAN_POINT('Ctrl Pts',(-1.0156297872271,-0.232742381310829,-0.0861971848975941));
#5895=CARTESIAN_POINT('Ctrl Pts',(-1.01358704779679,-0.223955109275652,
-0.106909345252087));
#5896=CARTESIAN_POINT('Ctrl Pts',(-1.00869718865384,-0.201072148666546,
-0.1465689792446));
#5897=CARTESIAN_POINT('Ctrl Pts',(-1.00492400591205,-0.181890537957859,
-0.169940289819232));
#5898=CARTESIAN_POINT('Ctrl Pts',(-0.998375294985966,-0.141695629206859,
-0.205111543747588));
#5899=CARTESIAN_POINT('Ctrl Pts',(-0.994830026707808,-0.11549207705665,
-0.221129100087819));
#5900=CARTESIAN_POINT('Ctrl Pts',(-0.991238884025248,-0.0742967091364495,
-0.236509675094874));
#5901=CARTESIAN_POINT('Ctrl Pts',(-0.990332542620729,-0.0609922781173484,
-0.24024064412003));
#5902=CARTESIAN_POINT('Ctrl Pts',(-0.989696097314,-0.0476300000000001,-0.242834539687907));
#5903=CARTESIAN_POINT('',(-0.871530771444223,-0.04763,-0.528110872004958));
#5904=CARTESIAN_POINT('Origin',(0.,-0.04763,0.));
#5905=CARTESIAN_POINT('',(-0.528110872004958,-0.04763,-0.871530771444223));
#5906=CARTESIAN_POINT('Ctrl Pts',(-0.871530771444223,-0.0476300000000001,
-0.528110872004958));
#5907=CARTESIAN_POINT('Ctrl Pts',(-0.87014664509073,-0.0609922781173484,
-0.530395067942936));
#5908=CARTESIAN_POINT('Ctrl Pts',(-0.868149331745851,-0.0742967091364494,
-0.533674141594226));
#5909=CARTESIAN_POINT('Ctrl Pts',(-0.85981294420286,-0.115492077056649,
-0.54708917182331));
#5910=CARTESIAN_POINT('Ctrl Pts',(-0.850993704737257,-0.141695629206859,
-0.560922177770136));
#5911=CARTESIAN_POINT('Ctrl Pts',(-0.830754510485543,-0.181890537957859,
-0.590422647829571));
#5912=CARTESIAN_POINT('Ctrl Pts',(-0.816896541396381,-0.201072148666546,
-0.609616703125488));
#5913=CARTESIAN_POINT('Ctrl Pts',(-0.792310597819928,-0.223955109275652,
-0.641117951819999));
#5914=CARTESIAN_POINT('Ctrl Pts',(-0.779109323683611,-0.232742381310829,
-0.657208095763053));
#5915=CARTESIAN_POINT('Ctrl Pts',(-0.750552691816205,-0.244234834628584,
-0.68964083160521));
#5916=CARTESIAN_POINT('Ctrl Pts',(-0.735185187071673,-0.246942143572133,
-0.705971972091755));
#5917=CARTESIAN_POINT('Ctrl Pts',(-0.705971972091754,-0.246942143572133,
-0.735185187071673));
#5918=CARTESIAN_POINT('Ctrl Pts',(-0.68964083160521,-0.244234834628584,
-0.750552691816206));
#5919=CARTESIAN_POINT('Ctrl Pts',(-0.657208095763052,-0.232742381310829,
-0.779109323683612));
#5920=CARTESIAN_POINT('Ctrl Pts',(-0.641117951819998,-0.223955109275652,
-0.792310597819928));
#5921=CARTESIAN_POINT('Ctrl Pts',(-0.609616703125488,-0.201072148666545,
-0.816896541396381));
#5922=CARTESIAN_POINT('Ctrl Pts',(-0.590422647829571,-0.181890537957859,
-0.830754510485543));
#5923=CARTESIAN_POINT('Ctrl Pts',(-0.560922177770136,-0.141695629206859,
-0.850993704737257));
#5924=CARTESIAN_POINT('Ctrl Pts',(-0.54708917182331,-0.115492077056649,
-0.85981294420286));
#5925=CARTESIAN_POINT('Ctrl Pts',(-0.533674141594226,-0.0742967091364494,
-0.868149331745852));
#5926=CARTESIAN_POINT('Ctrl Pts',(-0.530395067942936,-0.0609922781173484,
-0.870146645090731));
#5927=CARTESIAN_POINT('Ctrl Pts',(-0.528110872004958,-0.0476300000000001,
-0.871530771444223));
#5928=CARTESIAN_POINT('',(-0.242834539687906,-0.04763,-0.989696097314));
#5929=CARTESIAN_POINT('Origin',(0.,-0.04763,0.));
#5930=CARTESIAN_POINT('',(0.242834539687906,-0.04763,-0.989696097314));
#5931=CARTESIAN_POINT('Ctrl Pts',(-0.242834539687907,-0.04763,-0.989696097314));
#5932=CARTESIAN_POINT('Ctrl Pts',(-0.24024064412003,-0.0609922781173483,
-0.990332542620729));
#5933=CARTESIAN_POINT('Ctrl Pts',(-0.236509675094874,-0.0742967091364493,
-0.991238884025248));
#5934=CARTESIAN_POINT('Ctrl Pts',(-0.221129100087819,-0.115492077056649,
-0.994830026707808));
#5935=CARTESIAN_POINT('Ctrl Pts',(-0.205111543747588,-0.141695629206859,
-0.998375294985966));
#5936=CARTESIAN_POINT('Ctrl Pts',(-0.169940289819232,-0.181890537957859,
-1.00492400591205));
#5937=CARTESIAN_POINT('Ctrl Pts',(-0.1465689792446,-0.201072148666545,-1.00869718865384));
#5938=CARTESIAN_POINT('Ctrl Pts',(-0.106909345252087,-0.223955109275652,
-1.01358704779679));
#5939=CARTESIAN_POINT('Ctrl Pts',(-0.0861971848975942,-0.232742381310829,
-1.0156297872271));
#5940=CARTESIAN_POINT('Ctrl Pts',(-0.0430711894098823,-0.244234834628584,
-1.01837060663223));
#5941=CARTESIAN_POINT('Ctrl Pts',(-0.0206568624125606,-0.246942143572133,
-1.019052));
#5942=CARTESIAN_POINT('Ctrl Pts',(0.0206568624125607,-0.246942143572133,
-1.019052));
#5943=CARTESIAN_POINT('Ctrl Pts',(0.0430711894098824,-0.244234834628584,
-1.01837060663223));
#5944=CARTESIAN_POINT('Ctrl Pts',(0.0861971848975943,-0.232742381310829,
-1.0156297872271));
#5945=CARTESIAN_POINT('Ctrl Pts',(0.106909345252088,-0.223955109275652,
-1.01358704779679));
#5946=CARTESIAN_POINT('Ctrl Pts',(0.1465689792446,-0.201072148666545,-1.00869718865384));
#5947=CARTESIAN_POINT('Ctrl Pts',(0.169940289819232,-0.181890537957859,
-1.00492400591205));
#5948=CARTESIAN_POINT('Ctrl Pts',(0.205111543747588,-0.141695629206859,
-0.998375294985966));
#5949=CARTESIAN_POINT('Ctrl Pts',(0.221129100087819,-0.115492077056649,
-0.994830026707808));
#5950=CARTESIAN_POINT('Ctrl Pts',(0.236509675094874,-0.0742967091364493,
-0.991238884025248));
#5951=CARTESIAN_POINT('Ctrl Pts',(0.24024064412003,-0.0609922781173484,
-0.990332542620729));
#5952=CARTESIAN_POINT('Ctrl Pts',(0.242834539687907,-0.04763,-0.989696097314));
#5953=CARTESIAN_POINT('',(0.528110872004958,-0.04763,-0.871530771444223));
#5954=CARTESIAN_POINT('Origin',(0.,-0.04763,0.));
#5955=CARTESIAN_POINT('',(0.871530771444223,-0.04763,-0.528110872004958));
#5956=CARTESIAN_POINT('Ctrl Pts',(0.528110872004958,-0.0476300000000001,
-0.871530771444223));
#5957=CARTESIAN_POINT('Ctrl Pts',(0.530395067942936,-0.0609922781173484,
-0.870146645090731));
#5958=CARTESIAN_POINT('Ctrl Pts',(0.533674141594226,-0.0742967091364493,
-0.868149331745851));
#5959=CARTESIAN_POINT('Ctrl Pts',(0.54708917182331,-0.115492077056649,-0.85981294420286));
#5960=CARTESIAN_POINT('Ctrl Pts',(0.560922177770136,-0.141695629206859,
-0.850993704737257));
#5961=CARTESIAN_POINT('Ctrl Pts',(0.590422647829571,-0.181890537957859,
-0.830754510485543));
#5962=CARTESIAN_POINT('Ctrl Pts',(0.609616703125488,-0.201072148666545,
-0.816896541396381));
#5963=CARTESIAN_POINT('Ctrl Pts',(0.641117951819998,-0.223955109275652,
-0.792310597819928));
#5964=CARTESIAN_POINT('Ctrl Pts',(0.657208095763053,-0.232742381310829,
-0.779109323683612));
#5965=CARTESIAN_POINT('Ctrl Pts',(0.68964083160521,-0.244234834628584,-0.750552691816206));
#5966=CARTESIAN_POINT('Ctrl Pts',(0.705971972091755,-0.246942143572133,
-0.735185187071673));
#5967=CARTESIAN_POINT('Ctrl Pts',(0.735185187071673,-0.246942143572133,
-0.705971972091754));
#5968=CARTESIAN_POINT('Ctrl Pts',(0.750552691816206,-0.244234834628584,
-0.68964083160521));
#5969=CARTESIAN_POINT('Ctrl Pts',(0.779109323683612,-0.232742381310829,
-0.657208095763053));
#5970=CARTESIAN_POINT('Ctrl Pts',(0.792310597819928,-0.223955109275652,
-0.641117951819998));
#5971=CARTESIAN_POINT('Ctrl Pts',(0.816896541396381,-0.201072148666545,
-0.609616703125488));
#5972=CARTESIAN_POINT('Ctrl Pts',(0.830754510485543,-0.181890537957859,
-0.590422647829571));
#5973=CARTESIAN_POINT('Ctrl Pts',(0.850993704737257,-0.141695629206859,
-0.560922177770136));
#5974=CARTESIAN_POINT('Ctrl Pts',(0.85981294420286,-0.115492077056649,-0.54708917182331));
#5975=CARTESIAN_POINT('Ctrl Pts',(0.868149331745851,-0.0742967091364493,
-0.533674141594226));
#5976=CARTESIAN_POINT('Ctrl Pts',(0.870146645090731,-0.0609922781173484,
-0.530395067942936));
#5977=CARTESIAN_POINT('Ctrl Pts',(0.871530771444223,-0.0476300000000001,
-0.528110872004958));
#5978=CARTESIAN_POINT('',(0.989696097314,-0.04763,-0.242834539687906));
#5979=CARTESIAN_POINT('Origin',(0.,-0.04763,0.));
#5980=CARTESIAN_POINT('',(0.989696097314,-0.04763,0.242834539687906));
#5981=CARTESIAN_POINT('Ctrl Pts',(0.989696097314,-0.04763,-0.242834539687907));
#5982=CARTESIAN_POINT('Ctrl Pts',(0.990332542620729,-0.0609922781173483,
-0.24024064412003));
#5983=CARTESIAN_POINT('Ctrl Pts',(0.991238884025248,-0.0742967091364493,
-0.236509675094874));
#5984=CARTESIAN_POINT('Ctrl Pts',(0.994830026707808,-0.115492077056649,
-0.221129100087819));
#5985=CARTESIAN_POINT('Ctrl Pts',(0.998375294985966,-0.141695629206859,
-0.205111543747588));
#5986=CARTESIAN_POINT('Ctrl Pts',(1.00492400591205,-0.181890537957859,-0.169940289819232));
#5987=CARTESIAN_POINT('Ctrl Pts',(1.00869718865384,-0.201072148666545,-0.1465689792446));
#5988=CARTESIAN_POINT('Ctrl Pts',(1.01358704779679,-0.223955109275652,-0.106909345252087));
#5989=CARTESIAN_POINT('Ctrl Pts',(1.0156297872271,-0.232742381310829,-0.0861971848975942));
#5990=CARTESIAN_POINT('Ctrl Pts',(1.01837060663223,-0.244234834628584,-0.0430711894098823));
#5991=CARTESIAN_POINT('Ctrl Pts',(1.019052,-0.246942143572133,-0.0206568624125607));
#5992=CARTESIAN_POINT('Ctrl Pts',(1.019052,-0.246942143572133,0.0206568624125607));
#5993=CARTESIAN_POINT('Ctrl Pts',(1.01837060663223,-0.244234834628584,0.0430711894098823));
#5994=CARTESIAN_POINT('Ctrl Pts',(1.0156297872271,-0.232742381310829,0.0861971848975942));
#5995=CARTESIAN_POINT('Ctrl Pts',(1.01358704779679,-0.223955109275652,0.106909345252087));
#5996=CARTESIAN_POINT('Ctrl Pts',(1.00869718865384,-0.201072148666545,0.1465689792446));
#5997=CARTESIAN_POINT('Ctrl Pts',(1.00492400591205,-0.181890537957859,0.169940289819232));
#5998=CARTESIAN_POINT('Ctrl Pts',(0.998375294985966,-0.141695629206859,
0.205111543747588));
#5999=CARTESIAN_POINT('Ctrl Pts',(0.994830026707808,-0.115492077056649,
0.221129100087819));
#6000=CARTESIAN_POINT('Ctrl Pts',(0.991238884025248,-0.0742967091364492,
0.236509675094874));
#6001=CARTESIAN_POINT('Ctrl Pts',(0.990332542620729,-0.0609922781173483,
0.24024064412003));
#6002=CARTESIAN_POINT('Ctrl Pts',(0.989696097314,-0.04763,0.242834539687907));
#6003=CARTESIAN_POINT('Origin',(0.,-0.04763,0.));
#6004=CARTESIAN_POINT('Origin',(0.,-0.04763,0.));
#6005=CARTESIAN_POINT('',(0.238183666596899,-0.04763,0.951592097314));
#6006=CARTESIAN_POINT('Origin',(0.,-0.04763,0.));
#6007=CARTESIAN_POINT('Origin',(-1.94289029309402E-16,-0.04763,1.));
#6008=CARTESIAN_POINT('Origin',(-1.94289029309402E-16,0.,1.));
#6009=CARTESIAN_POINT('',(-0.2381836665969,-0.04763,0.951592097314));
#6010=CARTESIAN_POINT('Ctrl Pts',(-0.238183666596899,-0.0476299999999999,
0.951592097314));
#6011=CARTESIAN_POINT('Ctrl Pts',(-0.233157223576062,-0.0740444353928835,
0.952850216871763));
#6012=CARTESIAN_POINT('Ctrl Pts',(-0.223801617934946,-0.0999305678883309,
0.955173119738174));
#6013=CARTESIAN_POINT('Ctrl Pts',(-0.199966927975188,-0.142345102874864,
0.960411259488514));
#6014=CARTESIAN_POINT('Ctrl Pts',(-0.1868781821531,-0.159766064500479,0.963103647174702));
#6015=CARTESIAN_POINT('Ctrl Pts',(-0.15681442133453,-0.190326085855194,
0.968453058988463));
#6016=CARTESIAN_POINT('Ctrl Pts',(-0.139836317888043,-0.203463743702801,
0.971100730005489));
#6017=CARTESIAN_POINT('Ctrl Pts',(-0.104422493053067,-0.224161999508995,
0.975530745318961));
#6018=CARTESIAN_POINT('Ctrl Pts',(-0.0842175114474176,-0.232861760990032,
0.977553872336861));
#6019=CARTESIAN_POINT('Ctrl Pts',(-0.0421062857595701,-0.244251601209411,
0.980270995488453));
#6020=CARTESIAN_POINT('Ctrl Pts',(-0.0201990724523197,-0.246942143572133,
0.980948));
#6021=CARTESIAN_POINT('Ctrl Pts',(0.020199072452319,-0.246942143572133,
0.980948));
#6022=CARTESIAN_POINT('Ctrl Pts',(0.0421062857595694,-0.244251601209411,
0.980270995488454));
#6023=CARTESIAN_POINT('Ctrl Pts',(0.0842175114474169,-0.232861760990032,
0.977553872336861));
#6024=CARTESIAN_POINT('Ctrl Pts',(0.104422493053067,-0.224161999508995,
0.975530745318961));
#6025=CARTESIAN_POINT('Ctrl Pts',(0.139836317888042,-0.203463743702801,
0.971100730005489));
#6026=CARTESIAN_POINT('Ctrl Pts',(0.15681442133453,-0.190326085855194,0.968453058988463));
#6027=CARTESIAN_POINT('Ctrl Pts',(0.1868781821531,-0.15976606450048,0.963103647174702));
#6028=CARTESIAN_POINT('Ctrl Pts',(0.199966927975188,-0.142345102874864,
0.960411259488514));
#6029=CARTESIAN_POINT('Ctrl Pts',(0.223801617934945,-0.0999305678883309,
0.955173119738174));
#6030=CARTESIAN_POINT('Ctrl Pts',(0.233157223576061,-0.0740444353928835,
0.952850216871763));
#6031=CARTESIAN_POINT('Ctrl Pts',(0.238183666596899,-0.0476299999999999,
0.951592097314));
#6032=CARTESIAN_POINT('Origin',(-1.94289029309402E-16,-0.04763,1.));
#6033=CARTESIAN_POINT('Origin',(0.,-0.04763,0.));
#6034=CARTESIAN_POINT('',(-0.504455939115715,-0.04763,0.841298510752802));
#6035=CARTESIAN_POINT('Origin',(0.,-0.04763,0.));
#6036=CARTESIAN_POINT('Origin',(-0.707106781186548,-0.04763,0.707106781186547));
#6037=CARTESIAN_POINT('Origin',(-0.707106781186548,0.,0.707106781186547));
#6038=CARTESIAN_POINT('',(-0.841298510752802,-0.04763,0.504455939115715));
#6039=CARTESIAN_POINT('Ctrl Pts',(-0.841298510752802,-0.04763,0.504455939115715));
#6040=CARTESIAN_POINT('Ctrl Pts',(-0.838633903678357,-0.0740444353928835,
0.508899795931835));
#6041=CARTESIAN_POINT('Ctrl Pts',(-0.833661031856294,-0.0999305678883309,
0.517157748491652));
#6042=CARTESIAN_POINT('Ctrl Pts',(-0.820511285096538,-0.142345102874864,
0.537715343527944));
#6043=CARTESIAN_POINT('Ctrl Pts',(-0.813159949759,-0.159766064500479,0.548874290046456));
#6044=CARTESIAN_POINT('Ctrl Pts',(-0.795684265985089,-0.190326085855194,
0.573915184558107));
#6045=CARTESIAN_POINT('Ctrl Pts',(-0.78555112003688,-0.203463743702801,
0.587792702767295));
#6046=CARTESIAN_POINT('Ctrl Pts',(-0.763642258217233,-0.224161999508995,
0.615966552324775));
#6047=CARTESIAN_POINT('Ctrl Pts',(-0.750785745543687,-0.232861760990032,
0.631684198665438));
#6048=CARTESIAN_POINT('Ctrl Pts',(-0.722929908501543,-0.244251601209411,
0.663382628119203));
#6049=CARTESIAN_POINT('Ctrl Pts',(-0.707917883896095,-0.246942143572133,
0.679352081686668));
#6050=CARTESIAN_POINT('Ctrl Pts',(-0.679352081686668,-0.246942143572133,
0.707917883896095));
#6051=CARTESIAN_POINT('Ctrl Pts',(-0.663382628119203,-0.244251601209411,
0.722929908501544));
#6052=CARTESIAN_POINT('Ctrl Pts',(-0.631684198665438,-0.232861760990031,
0.750785745543687));
#6053=CARTESIAN_POINT('Ctrl Pts',(-0.615966552324775,-0.224161999508995,
0.763642258217233));
#6054=CARTESIAN_POINT('Ctrl Pts',(-0.587792702767295,-0.203463743702801,
0.78555112003688));
#6055=CARTESIAN_POINT('Ctrl Pts',(-0.573915184558107,-0.190326085855194,
0.795684265985088));
#6056=CARTESIAN_POINT('Ctrl Pts',(-0.548874290046456,-0.159766064500479,
0.813159949759));
#6057=CARTESIAN_POINT('Ctrl Pts',(-0.537715343527944,-0.142345102874864,
0.820511285096538));
#6058=CARTESIAN_POINT('Ctrl Pts',(-0.517157748491652,-0.0999305678883309,
0.833661031856294));
#6059=CARTESIAN_POINT('Ctrl Pts',(-0.508899795931835,-0.0740444353928835,
0.838633903678357));
#6060=CARTESIAN_POINT('Ctrl Pts',(-0.504455939115716,-0.04763,0.841298510752801));
#6061=CARTESIAN_POINT('Origin',(-0.707106781186548,-0.04763,0.707106781186547));
#6062=CARTESIAN_POINT('Origin',(0.,-0.04763,0.));
#6063=CARTESIAN_POINT('',(-0.951592097314,-0.04763,0.238183666596899));
#6064=CARTESIAN_POINT('Origin',(0.,-0.04763,0.));
#6065=CARTESIAN_POINT('Origin',(-1.,-0.04763,-1.11022302462516E-16));
#6066=CARTESIAN_POINT('Origin',(-1.,0.,-1.11022302462516E-16));
#6067=CARTESIAN_POINT('',(-0.951592097314,-0.04763,-0.2381836665969));
#6068=CARTESIAN_POINT('',(-0.980948,-0.246942143572133,1.08514323328844E-18));
#6069=CARTESIAN_POINT('Ctrl Pts',(-0.951592097314,-0.04763,-0.238183666596899));
#6070=CARTESIAN_POINT('Ctrl Pts',(-0.952850216871763,-0.0740444353928835,
-0.233157223576062));
#6071=CARTESIAN_POINT('Ctrl Pts',(-0.955173119738174,-0.0999305678883309,
-0.223801617934946));
#6072=CARTESIAN_POINT('Ctrl Pts',(-0.960411259488514,-0.142345102874864,
-0.199966927975188));
#6073=CARTESIAN_POINT('Ctrl Pts',(-0.963103647174702,-0.159766064500479,
-0.1868781821531));
#6074=CARTESIAN_POINT('Ctrl Pts',(-0.968453058988463,-0.190326085855194,
-0.15681442133453));
#6075=CARTESIAN_POINT('Ctrl Pts',(-0.971100730005489,-0.203463743702801,
-0.139836317888043));
#6076=CARTESIAN_POINT('Ctrl Pts',(-0.975530745318961,-0.224161999508995,
-0.104422493053067));
#6077=CARTESIAN_POINT('Ctrl Pts',(-0.977553872336861,-0.232861760990032,
-0.0842175114474175));
#6078=CARTESIAN_POINT('Ctrl Pts',(-0.980270995488453,-0.244251601209411,
-0.0421062857595699));
#6079=CARTESIAN_POINT('Ctrl Pts',(-0.980948,-0.246942143572133,-0.0201990724523195));
#6080=CARTESIAN_POINT('Ctrl Pts',(-0.980948,-0.246942143572133,-1.17961196366423E-16));
#6081=CARTESIAN_POINT('Origin',(-1.,-0.04763,-1.11022302462516E-16));
#6082=CARTESIAN_POINT('Ctrl Pts',(-0.980948,-0.246942143572133,-1.17961196366423E-16));
#6083=CARTESIAN_POINT('Ctrl Pts',(-0.980948,-0.246942143572133,0.0201990724523192));
#6084=CARTESIAN_POINT('Ctrl Pts',(-0.980270995488453,-0.244251601209411,
0.0421062857595695));
#6085=CARTESIAN_POINT('Ctrl Pts',(-0.977553872336861,-0.232861760990032,
0.0842175114474169));
#6086=CARTESIAN_POINT('Ctrl Pts',(-0.975530745318961,-0.224161999508995,
0.104422493053066));
#6087=CARTESIAN_POINT('Ctrl Pts',(-0.971100730005489,-0.203463743702801,
0.139836317888042));
#6088=CARTESIAN_POINT('Ctrl Pts',(-0.968453058988463,-0.190326085855194,
0.15681442133453));
#6089=CARTESIAN_POINT('Ctrl Pts',(-0.963103647174702,-0.15976606450048,
0.1868781821531));
#6090=CARTESIAN_POINT('Ctrl Pts',(-0.960411259488514,-0.142345102874864,
0.199966927975188));
#6091=CARTESIAN_POINT('Ctrl Pts',(-0.955173119738174,-0.099930567888331,
0.223801617934945));
#6092=CARTESIAN_POINT('Ctrl Pts',(-0.952850216871763,-0.0740444353928835,
0.233157223576061));
#6093=CARTESIAN_POINT('Ctrl Pts',(-0.951592097314,-0.04763,0.238183666596899));
#6094=CARTESIAN_POINT('Origin',(0.,-0.04763,0.));
#6095=CARTESIAN_POINT('',(-0.841298510752802,-0.04763,-0.504455939115715));
#6096=CARTESIAN_POINT('Origin',(0.,-0.04763,0.));
#6097=CARTESIAN_POINT('Origin',(-0.707106781186547,-0.04763,-0.707106781186548));
#6098=CARTESIAN_POINT('Origin',(-0.707106781186547,0.,-0.707106781186548));
#6099=CARTESIAN_POINT('',(-0.504455939115715,-0.04763,-0.841298510752802));
#6100=CARTESIAN_POINT('Ctrl Pts',(-0.504455939115715,-0.04763,-0.841298510752802));
#6101=CARTESIAN_POINT('Ctrl Pts',(-0.508899795931835,-0.0740444353928835,
-0.838633903678357));
#6102=CARTESIAN_POINT('Ctrl Pts',(-0.517157748491652,-0.0999305678883309,
-0.833661031856294));
#6103=CARTESIAN_POINT('Ctrl Pts',(-0.537715343527944,-0.142345102874864,
-0.820511285096538));
#6104=CARTESIAN_POINT('Ctrl Pts',(-0.548874290046456,-0.159766064500479,
-0.813159949759));
#6105=CARTESIAN_POINT('Ctrl Pts',(-0.573915184558107,-0.190326085855194,
-0.795684265985089));
#6106=CARTESIAN_POINT('Ctrl Pts',(-0.587792702767295,-0.203463743702801,
-0.78555112003688));
#6107=CARTESIAN_POINT('Ctrl Pts',(-0.615966552324775,-0.224161999508995,
-0.763642258217233));
#6108=CARTESIAN_POINT('Ctrl Pts',(-0.631684198665438,-0.232861760990032,
-0.750785745543687));
#6109=CARTESIAN_POINT('Ctrl Pts',(-0.663382628119203,-0.244251601209411,
-0.722929908501543));
#6110=CARTESIAN_POINT('Ctrl Pts',(-0.679352081686668,-0.246942143572133,
-0.707917883896095));
#6111=CARTESIAN_POINT('Ctrl Pts',(-0.707917883896095,-0.246942143572133,
-0.679352081686668));
#6112=CARTESIAN_POINT('Ctrl Pts',(-0.722929908501543,-0.244251601209411,
-0.663382628119203));
#6113=CARTESIAN_POINT('Ctrl Pts',(-0.750785745543687,-0.232861760990032,
-0.631684198665439));
#6114=CARTESIAN_POINT('Ctrl Pts',(-0.763642258217232,-0.224161999508995,
-0.615966552324775));
#6115=CARTESIAN_POINT('Ctrl Pts',(-0.78555112003688,-0.203463743702801,
-0.587792702767295));
#6116=CARTESIAN_POINT('Ctrl Pts',(-0.795684265985088,-0.190326085855194,
-0.573915184558107));
#6117=CARTESIAN_POINT('Ctrl Pts',(-0.813159949759,-0.15976606450048,-0.548874290046456));
#6118=CARTESIAN_POINT('Ctrl Pts',(-0.820511285096538,-0.142345102874864,
-0.537715343527944));
#6119=CARTESIAN_POINT('Ctrl Pts',(-0.833661031856294,-0.0999305678883311,
-0.517157748491652));
#6120=CARTESIAN_POINT('Ctrl Pts',(-0.838633903678357,-0.0740444353928836,
-0.508899795931835));
#6121=CARTESIAN_POINT('Ctrl Pts',(-0.841298510752801,-0.04763,-0.504455939115715));
#6122=CARTESIAN_POINT('Origin',(-0.707106781186547,-0.04763,-0.707106781186548));
#6123=CARTESIAN_POINT('Origin',(0.,-0.04763,0.));
#6124=CARTESIAN_POINT('',(-0.238183666596899,-0.04763,-0.951592097314));
#6125=CARTESIAN_POINT('Origin',(0.,-0.04763,0.));
#6126=CARTESIAN_POINT('Origin',(5.55111512312578E-17,-0.04763,-1.));
#6127=CARTESIAN_POINT('Origin',(5.55111512312578E-17,0.,-1.));
#6128=CARTESIAN_POINT('',(0.238183666596899,-0.04763,-0.951592097314));
#6129=CARTESIAN_POINT('Ctrl Pts',(0.238183666596899,-0.04763,-0.951592097314));
#6130=CARTESIAN_POINT('Ctrl Pts',(0.233157223576062,-0.0740444353928835,
-0.952850216871763));
#6131=CARTESIAN_POINT('Ctrl Pts',(0.223801617934946,-0.099930567888331,
-0.955173119738174));
#6132=CARTESIAN_POINT('Ctrl Pts',(0.199966927975188,-0.142345102874864,
-0.960411259488514));
#6133=CARTESIAN_POINT('Ctrl Pts',(0.1868781821531,-0.15976606450048,-0.963103647174702));
#6134=CARTESIAN_POINT('Ctrl Pts',(0.15681442133453,-0.190326085855194,-0.968453058988463));
#6135=CARTESIAN_POINT('Ctrl Pts',(0.139836317888042,-0.203463743702801,
-0.971100730005489));
#6136=CARTESIAN_POINT('Ctrl Pts',(0.104422493053067,-0.224161999508995,
-0.975530745318961));
#6137=CARTESIAN_POINT('Ctrl Pts',(0.0842175114474173,-0.232861760990032,
-0.977553872336861));
#6138=CARTESIAN_POINT('Ctrl Pts',(0.0421062857595698,-0.244251601209411,
-0.980270995488453));
#6139=CARTESIAN_POINT('Ctrl Pts',(0.0201990724523194,-0.246942143572133,
-0.980948));
#6140=CARTESIAN_POINT('Ctrl Pts',(-0.0201990724523193,-0.246942143572133,
-0.980948));
#6141=CARTESIAN_POINT('Ctrl Pts',(-0.0421062857595697,-0.244251601209411,
-0.980270995488453));
#6142=CARTESIAN_POINT('Ctrl Pts',(-0.0842175114474171,-0.232861760990032,
-0.977553872336861));
#6143=CARTESIAN_POINT('Ctrl Pts',(-0.104422493053067,-0.224161999508995,
-0.975530745318961));
#6144=CARTESIAN_POINT('Ctrl Pts',(-0.139836317888042,-0.203463743702801,
-0.971100730005489));
#6145=CARTESIAN_POINT('Ctrl Pts',(-0.15681442133453,-0.190326085855194,
-0.968453058988463));
#6146=CARTESIAN_POINT('Ctrl Pts',(-0.1868781821531,-0.15976606450048,-0.963103647174702));
#6147=CARTESIAN_POINT('Ctrl Pts',(-0.199966927975188,-0.142345102874864,
-0.960411259488514));
#6148=CARTESIAN_POINT('Ctrl Pts',(-0.223801617934945,-0.099930567888331,
-0.955173119738174));
#6149=CARTESIAN_POINT('Ctrl Pts',(-0.233157223576062,-0.0740444353928835,
-0.952850216871763));
#6150=CARTESIAN_POINT('Ctrl Pts',(-0.238183666596899,-0.0476299999999999,
-0.951592097314));
#6151=CARTESIAN_POINT('Origin',(5.55111512312578E-17,-0.04763,-1.));
#6152=CARTESIAN_POINT('Origin',(0.,-0.04763,0.));
#6153=CARTESIAN_POINT('',(0.504455939115715,-0.04763,-0.841298510752802));
#6154=CARTESIAN_POINT('Origin',(0.,-0.04763,0.));
#6155=CARTESIAN_POINT('Origin',(0.707106781186548,-0.04763,-0.707106781186547));
#6156=CARTESIAN_POINT('Origin',(0.707106781186548,0.,-0.707106781186547));
#6157=CARTESIAN_POINT('',(0.841298510752802,-0.04763,-0.504455939115715));
#6158=CARTESIAN_POINT('Ctrl Pts',(0.841298510752802,-0.04763,-0.504455939115715));
#6159=CARTESIAN_POINT('Ctrl Pts',(0.838633903678357,-0.0740444353928835,
-0.508899795931835));
#6160=CARTESIAN_POINT('Ctrl Pts',(0.833661031856294,-0.0999305678883309,
-0.517157748491652));
#6161=CARTESIAN_POINT('Ctrl Pts',(0.820511285096538,-0.142345102874864,
-0.537715343527944));
#6162=CARTESIAN_POINT('Ctrl Pts',(0.813159949759,-0.159766064500479,-0.548874290046456));
#6163=CARTESIAN_POINT('Ctrl Pts',(0.795684265985088,-0.190326085855194,
-0.573915184558107));
#6164=CARTESIAN_POINT('Ctrl Pts',(0.78555112003688,-0.203463743702801,-0.587792702767295));
#6165=CARTESIAN_POINT('Ctrl Pts',(0.763642258217233,-0.224161999508995,
-0.615966552324775));
#6166=CARTESIAN_POINT('Ctrl Pts',(0.750785745543687,-0.232861760990032,
-0.631684198665438));
#6167=CARTESIAN_POINT('Ctrl Pts',(0.722929908501543,-0.244251601209411,
-0.663382628119203));
#6168=CARTESIAN_POINT('Ctrl Pts',(0.707917883896095,-0.246942143572133,
-0.679352081686668));
#6169=CARTESIAN_POINT('Ctrl Pts',(0.679352081686668,-0.246942143572133,
-0.707917883896095));
#6170=CARTESIAN_POINT('Ctrl Pts',(0.663382628119203,-0.244251601209411,
-0.722929908501543));
#6171=CARTESIAN_POINT('Ctrl Pts',(0.631684198665438,-0.232861760990032,
-0.750785745543687));
#6172=CARTESIAN_POINT('Ctrl Pts',(0.615966552324775,-0.224161999508995,
-0.763642258217232));
#6173=CARTESIAN_POINT('Ctrl Pts',(0.587792702767295,-0.203463743702801,
-0.78555112003688));
#6174=CARTESIAN_POINT('Ctrl Pts',(0.573915184558107,-0.190326085855194,
-0.795684265985088));
#6175=CARTESIAN_POINT('Ctrl Pts',(0.548874290046456,-0.159766064500479,
-0.813159949759));
#6176=CARTESIAN_POINT('Ctrl Pts',(0.537715343527944,-0.142345102874864,
-0.820511285096538));
#6177=CARTESIAN_POINT('Ctrl Pts',(0.517157748491652,-0.099930567888331,
-0.833661031856294));
#6178=CARTESIAN_POINT('Ctrl Pts',(0.508899795931835,-0.0740444353928835,
-0.838633903678357));
#6179=CARTESIAN_POINT('Ctrl Pts',(0.504455939115715,-0.04763,-0.841298510752801));
#6180=CARTESIAN_POINT('Origin',(0.707106781186548,-0.04763,-0.707106781186547));
#6181=CARTESIAN_POINT('Origin',(0.,-0.166705,0.));
#6182=CARTESIAN_POINT('',(-0.980948,-0.28578,1.20131482833E-16));
#6183=CARTESIAN_POINT('Origin',(0.,-0.28578,0.));
#6184=CARTESIAN_POINT('',(-0.980948,-0.166705,1.20131482833E-16));
#6185=CARTESIAN_POINT('',(0.951592097314,-0.04763,0.238183666596899));
#6186=CARTESIAN_POINT('Origin',(0.,-0.04763,0.));
#6187=CARTESIAN_POINT('',(0.951592097314,-0.04763,-0.238183666596899));
#6188=CARTESIAN_POINT('Ctrl Pts',(0.951592097314,-0.04763,0.238183666596899));
#6189=CARTESIAN_POINT('Ctrl Pts',(0.952850216871763,-0.0740444353928835,
0.233157223576062));
#6190=CARTESIAN_POINT('Ctrl Pts',(0.955173119738174,-0.099930567888331,
0.223801617934945));
#6191=CARTESIAN_POINT('Ctrl Pts',(0.960411259488514,-0.142345102874864,
0.199966927975188));
#6192=CARTESIAN_POINT('Ctrl Pts',(0.963103647174702,-0.15976606450048,0.1868781821531));
#6193=CARTESIAN_POINT('Ctrl Pts',(0.968453058988463,-0.190326085855194,
0.15681442133453));
#6194=CARTESIAN_POINT('Ctrl Pts',(0.971100730005489,-0.203463743702801,
0.139836317888042));
#6195=CARTESIAN_POINT('Ctrl Pts',(0.975530745318961,-0.224161999508995,
0.104422493053067));
#6196=CARTESIAN_POINT('Ctrl Pts',(0.977553872336861,-0.232861760990032,
0.0842175114474172));
#6197=CARTESIAN_POINT('Ctrl Pts',(0.980270995488453,-0.244251601209411,
0.0421062857595697));
#6198=CARTESIAN_POINT('Ctrl Pts',(0.980948,-0.246942143572133,0.0201990724523194));
#6199=CARTESIAN_POINT('Ctrl Pts',(0.980948,-0.246942143572133,-0.0201990724523194));
#6200=CARTESIAN_POINT('Ctrl Pts',(0.980270995488453,-0.244251601209411,
-0.0421062857595697));
#6201=CARTESIAN_POINT('Ctrl Pts',(0.977553872336861,-0.232861760990032,
-0.0842175114474172));
#6202=CARTESIAN_POINT('Ctrl Pts',(0.975530745318961,-0.224161999508995,
-0.104422493053067));
#6203=CARTESIAN_POINT('Ctrl Pts',(0.971100730005489,-0.203463743702801,
-0.139836317888042));
#6204=CARTESIAN_POINT('Ctrl Pts',(0.968453058988463,-0.190326085855194,
-0.15681442133453));
#6205=CARTESIAN_POINT('Ctrl Pts',(0.963103647174702,-0.15976606450048,-0.1868781821531));
#6206=CARTESIAN_POINT('Ctrl Pts',(0.960411259488514,-0.142345102874864,
-0.199966927975188));
#6207=CARTESIAN_POINT('Ctrl Pts',(0.955173119738174,-0.099930567888331,
-0.223801617934945));
#6208=CARTESIAN_POINT('Ctrl Pts',(0.952850216871763,-0.0740444353928835,
-0.233157223576062));
#6209=CARTESIAN_POINT('Ctrl Pts',(0.951592097314,-0.0476299999999999,-0.238183666596899));
#6210=CARTESIAN_POINT('Origin',(0.,-0.04763,0.));
#6211=CARTESIAN_POINT('Origin',(0.,-0.04763,0.));
#6212=CARTESIAN_POINT('Origin',(1.,-0.04763,0.));
#6213=CARTESIAN_POINT('Origin',(1.,0.,0.));
#6214=CARTESIAN_POINT('Origin',(1.,-0.04763,0.));
#6215=CARTESIAN_POINT('Origin',(0.,-0.28578,0.));
#6216=CARTESIAN_POINT('Origin',(0.,-0.04763,0.));
#6217=CARTESIAN_POINT('',(0.,0.,0.));
#6218=CARTESIAN_POINT('Origin',(1.013815,0.445,0.));
#6219=CARTESIAN_POINT('',(-1.013815,0.445,-1.24156529467757E-16));
#6220=CARTESIAN_POINT('Origin',(0.,0.445,0.));
#6221=CARTESIAN_POINT('',(-0.991185,0.445,-1.21385153761287E-16));
#6222=CARTESIAN_POINT('Origin',(0.,0.445,0.));
#6223=CARTESIAN_POINT('Origin',(0.,0.4075,0.));
#6224=CARTESIAN_POINT('',(-1.013815,0.37,-1.24156529467757E-16));
#6225=CARTESIAN_POINT('Origin',(0.,0.37,0.));
#6226=CARTESIAN_POINT('',(-1.013815,0.4075,-1.24156529467757E-16));
#6227=CARTESIAN_POINT('Origin',(0.991185,0.37,0.));
#6228=CARTESIAN_POINT('',(-0.991185,0.37,-1.21385153761287E-16));
#6229=CARTESIAN_POINT('Origin',(0.,0.37,0.));
#6230=CARTESIAN_POINT('Origin',(0.,0.4075,0.));
#6231=CARTESIAN_POINT('',(-0.991185,0.4075,-1.21385153761287E-16));
#6232=CARTESIAN_POINT('Origin',(1.013815,-0.37,0.));
#6233=CARTESIAN_POINT('',(-1.013815,-0.37,-1.24156529467757E-16));
#6234=CARTESIAN_POINT('Origin',(0.,-0.37,0.));
#6235=CARTESIAN_POINT('',(-0.991185,-0.37,-1.21385153761287E-16));
#6236=CARTESIAN_POINT('Origin',(0.,-0.37,0.));
#6237=CARTESIAN_POINT('Origin',(0.,-0.4075,0.));
#6238=CARTESIAN_POINT('',(-1.013815,-0.445,-1.24156529467757E-16));
#6239=CARTESIAN_POINT('Origin',(0.,-0.445,0.));
#6240=CARTESIAN_POINT('',(-1.013815,-0.4075,-1.24156529467757E-16));
#6241=CARTESIAN_POINT('Origin',(0.991185,-0.445,0.));
#6242=CARTESIAN_POINT('',(-0.991185,-0.445,-1.21385153761287E-16));
#6243=CARTESIAN_POINT('Origin',(0.,-0.445,0.));
#6244=CARTESIAN_POINT('Origin',(0.,-0.4075,0.));
#6245=CARTESIAN_POINT('',(-0.991185,-0.4075,-1.21385153761287E-16));
#6246=CARTESIAN_POINT('',(0.,0.,0.));
#6247=CARTESIAN_POINT('',(0.,0.,0.));
#6248=CARTESIAN_POINT('',(0.,0.,0.));
#6249=CARTESIAN_POINT('',(0.,0.,0.));
#6250=CARTESIAN_POINT('',(0.,0.,0.));
#6251=CARTESIAN_POINT('',(0.,0.,0.));
#6252=CARTESIAN_POINT('Origin',(-1.23743686707646,-1.23743686707646,4.));
#6253=CARTESIAN_POINT('',(-1.61243686707646,-1.23743686707646,4.));
#6254=CARTESIAN_POINT('Origin',(-1.23743686707646,-1.23743686707646,4.));
#6255=CARTESIAN_POINT('',(-1.61243686707646,-1.23743686707646,4.4));
#6256=CARTESIAN_POINT('',(-1.61243686707646,-1.23743686707646,4.));
#6257=CARTESIAN_POINT('Origin',(-1.23743686707646,-1.23743686707646,4.4));
#6258=CARTESIAN_POINT('Origin',(-1.23743686707646,-1.23743686707646,4.));
#6259=CARTESIAN_POINT('',(-1.46243686707646,-1.23743686707646,4.));
#6260=CARTESIAN_POINT('Origin',(-1.23743686707646,-1.23743686707646,4.));
#6261=CARTESIAN_POINT('Origin',(-1.23743686707646,1.23743686707646,4.));
#6262=CARTESIAN_POINT('',(-1.61243686707646,1.23743686707646,4.));
#6263=CARTESIAN_POINT('Origin',(-1.23743686707646,1.23743686707646,4.));
#6264=CARTESIAN_POINT('',(-1.61243686707646,1.23743686707646,4.4));
#6265=CARTESIAN_POINT('',(-1.61243686707646,1.23743686707646,4.));
#6266=CARTESIAN_POINT('Origin',(-1.23743686707646,1.23743686707646,4.4));
#6267=CARTESIAN_POINT('Origin',(-1.23743686707646,1.23743686707646,4.));
#6268=CARTESIAN_POINT('',(-1.46243686707646,1.23743686707646,4.));
#6269=CARTESIAN_POINT('Origin',(-1.23743686707646,1.23743686707646,4.));
#6270=CARTESIAN_POINT('Origin',(1.23743686707646,1.23743686707646,4.));
#6271=CARTESIAN_POINT('',(0.862436867076458,1.23743686707646,4.));
#6272=CARTESIAN_POINT('Origin',(1.23743686707646,1.23743686707646,4.));
#6273=CARTESIAN_POINT('',(0.862436867076458,1.23743686707646,4.4));
#6274=CARTESIAN_POINT('',(0.862436867076458,1.23743686707646,4.));
#6275=CARTESIAN_POINT('Origin',(1.23743686707646,1.23743686707646,4.4));
#6276=CARTESIAN_POINT('Origin',(1.23743686707646,1.23743686707646,4.));
#6277=CARTESIAN_POINT('',(1.01243686707646,1.23743686707646,4.));
#6278=CARTESIAN_POINT('Origin',(1.23743686707646,1.23743686707646,4.));
#6279=CARTESIAN_POINT('Origin',(1.23743686707646,-1.23743686707646,4.));
#6280=CARTESIAN_POINT('',(0.862436867076458,-1.23743686707646,4.));
#6281=CARTESIAN_POINT('Origin',(1.23743686707646,-1.23743686707646,4.));
#6282=CARTESIAN_POINT('',(0.862436867076458,-1.23743686707646,4.4));
#6283=CARTESIAN_POINT('',(0.862436867076458,-1.23743686707646,4.));
#6284=CARTESIAN_POINT('Origin',(1.23743686707646,-1.23743686707646,4.4));
#6285=CARTESIAN_POINT('Origin',(1.23743686707646,-1.23743686707646,4.));
#6286=CARTESIAN_POINT('',(1.01243686707646,-1.23743686707646,4.));
#6287=CARTESIAN_POINT('Origin',(1.23743686707646,-1.23743686707646,4.));
#6288=CARTESIAN_POINT('Origin',(-1.23743686707646,-1.23743686707646,3.5));
#6289=CARTESIAN_POINT('',(-1.46243686707646,-1.23743686707646,3.6));
#6290=CARTESIAN_POINT('Origin',(-1.23743686707646,-1.23743686707646,3.6));
#6291=CARTESIAN_POINT('',(-1.46243686707646,-1.23743686707646,3.5));
#6292=CARTESIAN_POINT('Origin',(-1.23743686707646,1.23743686707646,3.5));
#6293=CARTESIAN_POINT('',(-1.46243686707646,1.23743686707646,3.6));
#6294=CARTESIAN_POINT('Origin',(-1.23743686707646,1.23743686707646,3.6));
#6295=CARTESIAN_POINT('',(-1.46243686707646,1.23743686707646,3.5));
#6296=CARTESIAN_POINT('Origin',(1.23743686707646,1.23743686707646,3.5));
#6297=CARTESIAN_POINT('',(1.01243686707646,1.23743686707646,3.6));
#6298=CARTESIAN_POINT('Origin',(1.23743686707646,1.23743686707646,3.6));
#6299=CARTESIAN_POINT('',(1.01243686707646,1.23743686707646,3.5));
#6300=CARTESIAN_POINT('Origin',(1.23743686707646,-1.23743686707646,3.5));
#6301=CARTESIAN_POINT('',(1.01243686707646,-1.23743686707646,3.6));
#6302=CARTESIAN_POINT('Origin',(1.23743686707646,-1.23743686707646,3.6));
#6303=CARTESIAN_POINT('',(1.01243686707646,-1.23743686707646,3.5));
#6304=CARTESIAN_POINT('Origin',(0.,0.,2.95));
#6305=CARTESIAN_POINT('',(-1.49,-1.82472373072956E-16,3.6));
#6306=CARTESIAN_POINT('Origin',(0.,0.,3.6));
#6307=CARTESIAN_POINT('',(-1.49,-1.82472373072956E-16,2.95));
#6308=CARTESIAN_POINT('',(-1.49,-1.82472373072956E-16,2.95));
#6309=CARTESIAN_POINT('Origin',(0.,0.,2.95));
#6310=CARTESIAN_POINT('Origin',(0.,0.,2.95));
#6311=CARTESIAN_POINT('',(-0.71,-8.69499227394621E-17,2.95));
#6312=CARTESIAN_POINT('Origin',(0.,0.,2.95));
#6313=CARTESIAN_POINT('Origin',(0.,0.,3.6));
#6314=CARTESIAN_POINT('',(-0.71,-8.69499227394621E-17,4.4));
#6315=CARTESIAN_POINT('Origin',(0.,0.,4.4));
#6316=CARTESIAN_POINT('',(-0.71,-8.69499227394621E-17,3.6));
#6317=CARTESIAN_POINT('Origin',(0.,0.,3.6));
#6318=CARTESIAN_POINT('',(-2.2,-2.69422295812418E-16,4.4));
#6319=CARTESIAN_POINT('Origin',(0.,0.,4.4));
#6320=CARTESIAN_POINT('',(-2.2,-2.69422295812418E-16,3.6));
#6321=CARTESIAN_POINT('',(-2.2,-2.69422295812418E-16,3.6));
#6322=CARTESIAN_POINT('Origin',(0.,0.,3.6));
#6323=CARTESIAN_POINT('Origin',(0.,0.,4.4));
#6324=CARTESIAN_POINT('Origin',(0.,0.,3.6));
#6325=CARTESIAN_POINT('',(0.,0.,0.));
#6326=CARTESIAN_POINT('Origin',(0.0866025403784439,-0.4,-0.15));
#6327=CARTESIAN_POINT('',(0.173205080756888,-0.4,0.));
#6328=CARTESIAN_POINT('',(0.0866025403784439,-0.4,-0.15));
#6329=CARTESIAN_POINT('',(0.173205080756888,-0.4,0.));
#6330=CARTESIAN_POINT('',(0.0866025403784439,-0.64,-0.15));
#6331=CARTESIAN_POINT('',(0.0866025403784439,-0.4,-0.15));
#6332=CARTESIAN_POINT('',(0.173205080756888,-0.64,0.));
#6333=CARTESIAN_POINT('',(0.173205080756888,-0.64,0.));
#6334=CARTESIAN_POINT('',(0.173205080756888,-0.4,0.));
#6335=CARTESIAN_POINT('Origin',(-0.0866025403784438,-0.4,-0.15));
#6336=CARTESIAN_POINT('',(-0.0866025403784438,-0.4,-0.15));
#6337=CARTESIAN_POINT('',(0.0866025403784439,-0.4,-0.15));
#6338=CARTESIAN_POINT('',(-0.0866025403784438,-0.64,-0.15));
#6339=CARTESIAN_POINT('',(-0.0866025403784438,-0.4,-0.15));
#6340=CARTESIAN_POINT('',(0.0866025403784439,-0.64,-0.15));
#6341=CARTESIAN_POINT('Origin',(-0.173205080756888,-0.4,-2.77555756156289E-17));
#6342=CARTESIAN_POINT('',(-0.173205080756888,-0.4,-2.12115047744981E-17));
#6343=CARTESIAN_POINT('',(-0.0866025403784438,-0.4,-0.15));
#6344=CARTESIAN_POINT('',(-0.173205080756888,-0.64,-2.77555756156289E-17));
#6345=CARTESIAN_POINT('',(-0.173205080756888,-0.4,-2.12115047744981E-17));
#6346=CARTESIAN_POINT('',(-0.0866025403784438,-0.64,-0.15));
#6347=CARTESIAN_POINT('Origin',(-0.0866025403784439,-0.4,0.15));
#6348=CARTESIAN_POINT('',(-0.0866025403784439,-0.4,0.15));
#6349=CARTESIAN_POINT('',(-0.173205080756888,-0.4,-2.12115047744981E-17));
#6350=CARTESIAN_POINT('',(-0.0866025403784439,-0.64,0.15));
#6351=CARTESIAN_POINT('',(-0.0866025403784439,-0.4,0.15));
#6352=CARTESIAN_POINT('',(-0.173205080756888,-0.64,-2.12115047744981E-17));
#6353=CARTESIAN_POINT('Origin',(0.0866025403784439,-0.4,0.15));
#6354=CARTESIAN_POINT('',(0.0866025403784439,-0.4,0.15));
#6355=CARTESIAN_POINT('',(-0.0866025403784439,-0.4,0.15));
#6356=CARTESIAN_POINT('',(0.0866025403784439,-0.64,0.15));
#6357=CARTESIAN_POINT('',(0.0866025403784439,-0.4,0.15));
#6358=CARTESIAN_POINT('',(-0.0866025403784439,-0.64,0.15));
#6359=CARTESIAN_POINT('Origin',(0.173205080756888,-0.4,0.));
#6360=CARTESIAN_POINT('',(0.0866025403784439,-0.4,0.15));
#6361=CARTESIAN_POINT('',(0.0866025403784439,-0.64,0.15));
#6362=CARTESIAN_POINT('Origin',(0.,-0.4,-2.77555756156289E-17));
#6363=CARTESIAN_POINT('Origin',(0.,-0.64,-2.77555756156289E-17));
#6364=CARTESIAN_POINT('Origin',(0.,-1.,0.));
#6365=CARTESIAN_POINT('',(-0.1954,-1.,2.39295984553393E-17));
#6366=CARTESIAN_POINT('Origin',(0.,-1.,0.));
#6367=CARTESIAN_POINT('Origin',(0.3,0.4,0.));
#6368=CARTESIAN_POINT('',(-0.3,0.4,-3.67394039744206E-17));
#6369=CARTESIAN_POINT('Origin',(0.,0.4,0.));
#6370=CARTESIAN_POINT('Origin',(0.,0.375,0.));
#6371=CARTESIAN_POINT('',(-0.35,0.35,-4.28626379701573E-17));
#6372=CARTESIAN_POINT('Origin',(0.,0.35,0.));
#6373=CARTESIAN_POINT('',(-0.325,0.375,-3.9801020972289E-17));
#6374=CARTESIAN_POINT('Origin',(0.,0.19,0.));
#6375=CARTESIAN_POINT('',(-0.35,0.03,-4.28626379701574E-17));
#6376=CARTESIAN_POINT('Origin',(0.,0.03,0.));
#6377=CARTESIAN_POINT('',(-0.35,0.19,-4.28626379701574E-17));
#6378=CARTESIAN_POINT('Origin',(0.,0.0149999999999999,0.));
#6379=CARTESIAN_POINT('',(-0.32,-3.29597460435593E-17,-3.91886975727153E-17));
#6380=CARTESIAN_POINT('Origin',(0.,0.,0.));
#6381=CARTESIAN_POINT('',(-0.335,0.0149999999999999,-4.10256677714363E-17));
#6382=CARTESIAN_POINT('Origin',(0.22,0.,0.));
#6383=CARTESIAN_POINT('',(-0.22,-6.93889390390723E-18,-2.69422295812418E-17));
#6384=CARTESIAN_POINT('Origin',(0.,0.,0.));
#6385=CARTESIAN_POINT('Origin',(0.,-0.02,0.));
#6386=CARTESIAN_POINT('',(-0.1954,-0.0492,2.39295984553393E-17));
#6387=CARTESIAN_POINT('Origin',(0.,-0.0492,0.));
#6388=CARTESIAN_POINT('',(-0.21,-0.02,-2.57175827820944E-17));
#6389=CARTESIAN_POINT('Origin',(0.,-0.8,0.));
#6390=CARTESIAN_POINT('',(-0.1954,-0.8,-2.39295984553393E-17));
#6391=CARTESIAN_POINT('',(0.,0.,0.));
#6392=CARTESIAN_POINT('',(0.,0.,0.));
#6393=CARTESIAN_POINT('',(0.,0.,0.));
#6394=CARTESIAN_POINT('',(0.,0.,2.5));
#6395=CARTESIAN_POINT('',(1.76776695296637,1.76776695296637,1.8));
#6396=CARTESIAN_POINT('',(-1.76776695296637,1.76776695296637,1.8));
#6397=CARTESIAN_POINT('',(-1.76776695296637,-1.76776695296637,1.8));
#6398=CARTESIAN_POINT('',(1.76776695296637,-1.76776695296637,1.8));
#6399=CARTESIAN_POINT('',(1.23743686707646,1.23743686707646,4.));
#6400=CARTESIAN_POINT('',(-1.23743686707646,1.23743686707646,4.));
#6401=CARTESIAN_POINT('',(-1.23743686707646,-1.23743686707646,4.));
#6402=CARTESIAN_POINT('',(1.23743686707646,-1.23743686707646,4.));
#6403=CARTESIAN_POINT('',(8.,0.,0.));
#6404=CARTESIAN_POINT('',(8.,0.,0.));
#6405=CARTESIAN_POINT('',(8.,0.,2.5));
#6406=CARTESIAN_POINT('',(9.76776695296637,1.76776695296637,1.8));
#6407=CARTESIAN_POINT('',(6.23223304703363,1.76776695296637,1.8));
#6408=CARTESIAN_POINT('',(6.23223304703363,-1.76776695296637,1.8));
#6409=CARTESIAN_POINT('',(9.76776695296637,-1.76776695296637,1.8));
#6410=CARTESIAN_POINT('',(9.23743686707646,1.23743686707646,4.));
#6411=CARTESIAN_POINT('',(6.76256313292354,1.23743686707646,4.));
#6412=CARTESIAN_POINT('',(6.76256313292354,-1.23743686707646,4.));
#6413=CARTESIAN_POINT('',(9.23743686707646,-1.23743686707646,4.));
#6414=CARTESIAN_POINT('',(0.,0.,0.));
#6415=CARTESIAN_POINT('',(0.,0.,0.));
#6416=CARTESIAN_POINT('Origin',(10.,3.46410161513775,7.55));
#6417=CARTESIAN_POINT('',(9.2,4.06410161513775,8.35));
#6418=CARTESIAN_POINT('',(9.2,4.06410161513775,7.55));
#6419=CARTESIAN_POINT('',(9.2,4.06410161513775,7.55));
#6420=CARTESIAN_POINT('',(9.2,2.86410161513775,8.35));
#6421=CARTESIAN_POINT('Origin',(10.,3.46410161513775,8.35));
#6422=CARTESIAN_POINT('',(9.2,2.86410161513775,7.55));
#6423=CARTESIAN_POINT('',(9.2,2.86410161513775,7.55));
#6424=CARTESIAN_POINT('Origin',(10.,3.46410161513775,7.55));
#6425=CARTESIAN_POINT('Origin',(10.,4.06410161513775,7.55));
#6426=CARTESIAN_POINT('',(2.8,4.06410161513775,7.55));
#6427=CARTESIAN_POINT('',(2.,4.06410161513775,7.55));
#6428=CARTESIAN_POINT('',(2.8,4.06410161513775,8.35));
#6429=CARTESIAN_POINT('',(2.8,4.06410161513775,7.55));
#6430=CARTESIAN_POINT('',(2.,4.06410161513775,8.35));
#6431=CARTESIAN_POINT('Origin',(2.,3.46410161513775,7.55));
#6432=CARTESIAN_POINT('',(2.8,2.86410161513775,7.55));
#6433=CARTESIAN_POINT('',(10.,2.86410161513775,7.55));
#6434=CARTESIAN_POINT('Origin',(2.,3.46410161513775,7.55));
#6435=CARTESIAN_POINT('',(9.3,3.46410161513775,7.55));
#6436=CARTESIAN_POINT('Origin',(10.,3.46410161513775,7.55));
#6437=CARTESIAN_POINT('',(1.3,3.46410161513775,7.55));
#6438=CARTESIAN_POINT('Origin',(2.,3.46410161513775,7.55));
#6439=CARTESIAN_POINT('Origin',(10.,3.46410161513775,5.7));
#6440=CARTESIAN_POINT('',(9.3,3.46410161513775,5.7));
#6441=CARTESIAN_POINT('Origin',(10.,3.46410161513775,5.7));
#6442=CARTESIAN_POINT('',(9.5,3.46410161513775,5.7));
#6443=CARTESIAN_POINT('Origin',(10.,3.46410161513775,5.7));
#6444=CARTESIAN_POINT('Origin',(10.,3.46410161513775,5.7));
#6445=CARTESIAN_POINT('',(9.3,3.46410161513775,5.7));
#6446=CARTESIAN_POINT('Origin',(10.,3.46410161513775,3.75));
#6447=CARTESIAN_POINT('',(9.5,3.46410161513775,3.75));
#6448=CARTESIAN_POINT('',(9.5,3.46410161513775,3.75));
#6449=CARTESIAN_POINT('Origin',(10.,3.46410161513775,3.75));
#6450=CARTESIAN_POINT('Origin',(10.,3.46410161513775,3.75));
#6451=CARTESIAN_POINT('Origin',(2.,2.86410161513775,7.55));
#6452=CARTESIAN_POINT('',(2.8,2.86410161513775,8.35));
#6453=CARTESIAN_POINT('',(10.,2.86410161513775,8.35));
#6454=CARTESIAN_POINT('',(2.8,2.86410161513775,7.55));
#6455=CARTESIAN_POINT('Origin',(2.,3.46410161513775,7.55));
#6456=CARTESIAN_POINT('Origin',(2.,3.46410161513775,8.35));
#6457=CARTESIAN_POINT('Origin',(2.,3.46410161513775,5.7));
#6458=CARTESIAN_POINT('',(1.3,3.46410161513775,5.7));
#6459=CARTESIAN_POINT('Origin',(2.,3.46410161513775,5.7));
#6460=CARTESIAN_POINT('',(1.5,3.46410161513775,5.7));
#6461=CARTESIAN_POINT('Origin',(2.,3.46410161513775,5.7));
#6462=CARTESIAN_POINT('Origin',(2.,3.46410161513775,5.7));
#6463=CARTESIAN_POINT('',(1.3,3.46410161513775,5.7));
#6464=CARTESIAN_POINT('Origin',(2.,3.46410161513775,3.75));
#6465=CARTESIAN_POINT('',(1.5,3.46410161513775,3.75));
#6466=CARTESIAN_POINT('',(1.5,3.46410161513775,3.75));
#6467=CARTESIAN_POINT('Origin',(2.,3.46410161513775,3.75));
#6468=CARTESIAN_POINT('Origin',(2.,3.46410161513775,8.35));
#6469=CARTESIAN_POINT('Origin',(2.,3.46410161513775,3.75));
#6470=CARTESIAN_POINT('',(0.,0.,0.));
#6471=CARTESIAN_POINT('Origin',(0.,0.,1.8));
#6472=CARTESIAN_POINT('',(-0.505,-6.18446633569413E-17,2.05));
#6473=CARTESIAN_POINT('Origin',(0.,0.,2.05));
#6474=CARTESIAN_POINT('',(-0.505,-6.18446633569413E-17,1.8));
#6475=CARTESIAN_POINT('',(-0.505,-6.18446633569413E-17,1.8));
#6476=CARTESIAN_POINT('Origin',(0.,0.,1.8));
#6477=CARTESIAN_POINT('Origin',(0.,0.,1.8));
#6478=CARTESIAN_POINT('',(-0.7,-8.57252759403147E-17,2.05));
#6479=CARTESIAN_POINT('Origin',(0.,0.,2.05));
#6480=CARTESIAN_POINT('',(-0.7,-8.57252759403147E-17,1.8));
#6481=CARTESIAN_POINT('',(-0.7,-8.57252759403147E-17,1.8));
#6482=CARTESIAN_POINT('Origin',(0.,0.,1.8));
#6483=CARTESIAN_POINT('Origin',(0.,0.,2.05));
#6484=CARTESIAN_POINT('Origin',(0.,0.,1.8));
#6485=CARTESIAN_POINT('',(0.,0.,0.));
#6486=CARTESIAN_POINT('Origin',(0.49,0.,1.4));
#6487=CARTESIAN_POINT('',(0.49,0.122167917228706,1.28909463493591));
#6488=CARTESIAN_POINT('',(0.49,0.122167917228706,1.51090536506409));
#6489=CARTESIAN_POINT('',(0.49,0.122167917228706,1.));
#6490=CARTESIAN_POINT('Origin',(0.49,0.,1.4));
#6491=CARTESIAN_POINT('Origin',(0.49,0.,1.4));
#6492=CARTESIAN_POINT('',(0.49,-0.122167917228706,1.28909463493591));
#6493=CARTESIAN_POINT('Ctrl Pts',(0.49,-0.122167917228706,1.28909463493591));
#6494=CARTESIAN_POINT('Ctrl Pts',(0.490448531679987,-0.120368913626296,
1.28711294069536));
#6495=CARTESIAN_POINT('Ctrl Pts',(0.490895245371685,-0.118534896565231,
1.28518965877367));
#6496=CARTESIAN_POINT('Ctrl Pts',(0.494795015531646,-0.102111993019358,
1.2687667552278));
#6497=CARTESIAN_POINT('Ctrl Pts',(0.498442514607594,-0.0836597150224318,
1.25609154388858));
#6498=CARTESIAN_POINT('Ctrl Pts',(0.50357781976106,-0.0430495960471595,
1.23920409039234));
#6499=CARTESIAN_POINT('Ctrl Pts',(0.505,-0.020880094330741,1.235));
#6500=CARTESIAN_POINT('Ctrl Pts',(0.505,0.020880094330741,1.235));
#6501=CARTESIAN_POINT('Ctrl Pts',(0.50357781976106,0.0430495960471595,1.23920409039234));
#6502=CARTESIAN_POINT('Ctrl Pts',(0.498442514607594,0.0836597150224318,
1.25609154388858));
#6503=CARTESIAN_POINT('Ctrl Pts',(0.494795015531646,0.102111993019358,1.2687667552278));
#6504=CARTESIAN_POINT('Ctrl Pts',(0.490895245371684,0.118534896565231,1.28518965877367));
#6505=CARTESIAN_POINT('Ctrl Pts',(0.490448531679987,0.120368913626296,1.28711294069536));
#6506=CARTESIAN_POINT('Ctrl Pts',(0.49,0.122167917228706,1.28909463493591));
#6507=CARTESIAN_POINT('',(0.49,-0.122167917228706,1.51090536506409));
#6508=CARTESIAN_POINT('Origin',(0.49,0.,1.4));
#6509=CARTESIAN_POINT('',(0.505,-1.70422299968729E-17,1.565));
#6510=CARTESIAN_POINT('Ctrl Pts',(0.505,-6.93889390390723E-18,1.565));
#6511=CARTESIAN_POINT('Ctrl Pts',(0.505,-0.020880094330741,1.565));
#6512=CARTESIAN_POINT('Ctrl Pts',(0.50357781976106,-0.0430495960471595,
1.56079590960766));
#6513=CARTESIAN_POINT('Ctrl Pts',(0.498442514607594,-0.0836597150224318,
1.54390845611142));
#6514=CARTESIAN_POINT('Ctrl Pts',(0.494795015531646,-0.102111993019358,
1.5312332447722));
#6515=CARTESIAN_POINT('Ctrl Pts',(0.490895245371684,-0.118534896565231,
1.51481034122633));
#6516=CARTESIAN_POINT('Ctrl Pts',(0.490448531679987,-0.120368913626296,
1.51288705930464));
#6517=CARTESIAN_POINT('Ctrl Pts',(0.49,-0.122167917228706,1.51090536506409));
#6518=CARTESIAN_POINT('',(0.9,-2.02066721859313E-17,1.565));
#6519=CARTESIAN_POINT('',(0.49,-2.02066721859313E-17,1.565));
#6520=CARTESIAN_POINT('',(0.884745726183518,0.165,1.4));
#6521=CARTESIAN_POINT('Ctrl Pts',(0.884745726183518,0.165,1.4));
#6522=CARTESIAN_POINT('Ctrl Pts',(0.884745726183518,0.165,1.37923124059256));
#6523=CARTESIAN_POINT('Ctrl Pts',(0.885552759505264,0.160839719007584,1.35711110492666));
#6524=CARTESIAN_POINT('Ctrl Pts',(0.888448648150043,0.143986470216691,1.31647293736623));
#6525=CARTESIAN_POINT('Ctrl Pts',(0.890493604851638,0.131295993814186,1.29795075602263));
#6526=CARTESIAN_POINT('Ctrl Pts',(0.89431723432394,0.102049819008125,1.26870458121656));
#6527=CARTESIAN_POINT('Ctrl Pts',(0.896347088899543,0.0835273920906824,
1.25601365401642));
#6528=CARTESIAN_POINT('Ctrl Pts',(0.899208271860583,0.0428883760934127,
1.23916007816136));
#6529=CARTESIAN_POINT('Ctrl Pts',(0.9,0.0207679427235068,1.235));
#6530=CARTESIAN_POINT('Ctrl Pts',(0.9,-0.0207679427235068,1.235));
#6531=CARTESIAN_POINT('Ctrl Pts',(0.899208271860583,-0.0428883760934127,
1.23916007816136));
#6532=CARTESIAN_POINT('Ctrl Pts',(0.896347088899543,-0.0835273920906823,
1.25601365401642));
#6533=CARTESIAN_POINT('Ctrl Pts',(0.89431723432394,-0.102049819008125,1.26870458121656));
#6534=CARTESIAN_POINT('Ctrl Pts',(0.890493604851638,-0.131295993814186,
1.29795075602263));
#6535=CARTESIAN_POINT('Ctrl Pts',(0.888448648150043,-0.143986470216691,
1.31647293736623));
#6536=CARTESIAN_POINT('Ctrl Pts',(0.885552759505264,-0.160839719007584,
1.35711110492666));
#6537=CARTESIAN_POINT('Ctrl Pts',(0.884745726183518,-0.165,1.37923124059256));
#6538=CARTESIAN_POINT('Ctrl Pts',(0.884745726183518,-0.165,1.42076875940744));
#6539=CARTESIAN_POINT('Ctrl Pts',(0.885552759505264,-0.160839719007584,
1.44288889507334));
#6540=CARTESIAN_POINT('Ctrl Pts',(0.888448648150043,-0.14398647021669,1.48352706263377));
#6541=CARTESIAN_POINT('Ctrl Pts',(0.890493604851638,-0.131295993814186,
1.50204924397737));
#6542=CARTESIAN_POINT('Ctrl Pts',(0.89431723432394,-0.102049819008125,1.53129541878344));
#6543=CARTESIAN_POINT('Ctrl Pts',(0.896347088899543,-0.0835273920906824,
1.54398634598358));
#6544=CARTESIAN_POINT('Ctrl Pts',(0.899208271860583,-0.0428883760934128,
1.56083992183864));
#6545=CARTESIAN_POINT('Ctrl Pts',(0.9,-0.0207679427235068,1.565));
#6546=CARTESIAN_POINT('Ctrl Pts',(0.9,-6.93889390390723E-18,1.565));
#6547=CARTESIAN_POINT('Ctrl Pts',(0.9,-3.46944695195361E-17,1.565));
#6548=CARTESIAN_POINT('Ctrl Pts',(0.9,0.0207679427235068,1.565));
#6549=CARTESIAN_POINT('Ctrl Pts',(0.899208271860583,0.0428883760934127,
1.56083992183864));
#6550=CARTESIAN_POINT('Ctrl Pts',(0.896347088899543,0.0835273920906824,
1.54398634598358));
#6551=CARTESIAN_POINT('Ctrl Pts',(0.89431723432394,0.102049819008125,1.53129541878344));
#6552=CARTESIAN_POINT('Ctrl Pts',(0.890493604851638,0.131295993814186,1.50204924397737));
#6553=CARTESIAN_POINT('Ctrl Pts',(0.888448648150043,0.143986470216691,1.48352706263377));
#6554=CARTESIAN_POINT('Ctrl Pts',(0.885552759505264,0.160839719007584,1.44288889507334));
#6555=CARTESIAN_POINT('Ctrl Pts',(0.884745726183518,0.165,1.42076875940744));
#6556=CARTESIAN_POINT('Ctrl Pts',(0.884745726183518,0.165,1.4));
#6557=CARTESIAN_POINT('Ctrl Pts',(0.49,0.122167917228706,1.51090536506409));
#6558=CARTESIAN_POINT('Ctrl Pts',(0.490448531679987,0.120368913626296,1.51288705930464));
#6559=CARTESIAN_POINT('Ctrl Pts',(0.490895245371685,0.118534896565231,1.51481034122633));
#6560=CARTESIAN_POINT('Ctrl Pts',(0.494795015531646,0.102111993019358,1.5312332447722));
#6561=CARTESIAN_POINT('Ctrl Pts',(0.498442514607594,0.0836597150224318,
1.54390845611142));
#6562=CARTESIAN_POINT('Ctrl Pts',(0.50357781976106,0.0430495960471594,1.56079590960766));
#6563=CARTESIAN_POINT('Ctrl Pts',(0.505,0.020880094330741,1.565));
#6564=CARTESIAN_POINT('Ctrl Pts',(0.505,0.,1.565));
#6565=CARTESIAN_POINT('Origin',(0.49,0.,1.4));
#6566=CARTESIAN_POINT('',(0.49,-0.122167917228706,1.));
#6567=CARTESIAN_POINT('Origin',(0.,0.,1.));
#6568=CARTESIAN_POINT('',(-0.505,-6.18446633569413E-17,1.8));
#6569=CARTESIAN_POINT('Origin',(0.,0.,1.8));
#6570=CARTESIAN_POINT('',(-0.505,-6.18446633569413E-17,1.));
#6571=CARTESIAN_POINT('',(-0.505,-6.18446633569413E-17,1.));
#6572=CARTESIAN_POINT('Origin',(0.,0.,1.));
#6573=CARTESIAN_POINT('Origin',(0.,0.,1.));
#6574=CARTESIAN_POINT('',(-0.9,-1.10218211923262E-16,1.8));
#6575=CARTESIAN_POINT('Origin',(0.,0.,1.8));
#6576=CARTESIAN_POINT('',(-0.9,-1.10218211923262E-16,1.));
#6577=CARTESIAN_POINT('',(-0.9,-1.10218211923262E-16,1.));
#6578=CARTESIAN_POINT('Origin',(0.,0.,1.));
#6579=CARTESIAN_POINT('Origin',(0.,0.,1.8));
#6580=CARTESIAN_POINT('Origin',(0.,0.,1.));
#6581=CARTESIAN_POINT('',(0.,0.,0.));
#6582=CARTESIAN_POINT('Origin',(0.,-0.4,0.));
#6583=CARTESIAN_POINT('',(-0.1954,-0.4,2.39295984553393E-17));
#6584=CARTESIAN_POINT('Origin',(0.,-0.4,0.));
#6585=CARTESIAN_POINT('Origin',(0.0577350269189626,0.,-0.1));
#6586=CARTESIAN_POINT('',(0.0577350269189626,0.,-0.1));
#6587=CARTESIAN_POINT('',(0.115470053837925,0.,0.));
#6588=CARTESIAN_POINT('',(0.0934187836487032,0.,-0.0381939203391614));
#6589=CARTESIAN_POINT('',(0.0577350269189626,-0.2,-0.1));
#6590=CARTESIAN_POINT('',(0.0577350269189626,0.,-0.1));
#6591=CARTESIAN_POINT('',(0.115470053837925,-0.2,0.));
#6592=CARTESIAN_POINT('',(0.115470053837925,-0.2,0.));
#6593=CARTESIAN_POINT('',(0.115470053837925,0.,0.));
#6594=CARTESIAN_POINT('Origin',(-0.0577350269189626,0.,-0.1));
#6595=CARTESIAN_POINT('',(-0.0577350269189626,0.,-0.1));
#6596=CARTESIAN_POINT('',(0.0561324865405187,0.,-0.1));
#6597=CARTESIAN_POINT('',(-0.0577350269189626,-0.2,-0.1));
#6598=CARTESIAN_POINT('',(-0.0577350269189626,0.,-0.1));
#6599=CARTESIAN_POINT('',(0.0577350269189626,-0.2,-0.1));
#6600=CARTESIAN_POINT('Origin',(-0.115470053837925,0.,-1.38777878078145E-17));
#6601=CARTESIAN_POINT('',(-0.115470053837925,0.,-1.41410031829988E-17));
#6602=CARTESIAN_POINT('',(-0.0797862971081845,0.,-0.0618060796608387));
#6603=CARTESIAN_POINT('',(-0.115470053837925,-0.2,-1.38777878078145E-17));
#6604=CARTESIAN_POINT('',(-0.115470053837925,0.,-1.41410031829988E-17));
#6605=CARTESIAN_POINT('',(-0.0577350269189626,-0.2,-0.1));
#6606=CARTESIAN_POINT('Origin',(-0.0577350269189626,0.,0.1));
#6607=CARTESIAN_POINT('',(-0.0577350269189626,0.,0.1));
#6608=CARTESIAN_POINT('',(-0.0509187836487033,0.,0.111806079660839));
#6609=CARTESIAN_POINT('',(-0.0577350269189626,-0.2,0.1));
#6610=CARTESIAN_POINT('',(-0.0577350269189626,0.,0.1));
#6611=CARTESIAN_POINT('',(-0.115470053837925,-0.2,-1.41410031829988E-17));
#6612=CARTESIAN_POINT('Origin',(0.0577350269189626,0.,0.1));
#6613=CARTESIAN_POINT('',(0.0577350269189626,0.,0.1));
#6614=CARTESIAN_POINT('',(0.113867513459481,0.,0.1));
#6615=CARTESIAN_POINT('',(0.0577350269189626,-0.2,0.1));
#6616=CARTESIAN_POINT('',(0.0577350269189626,0.,0.1));
#6617=CARTESIAN_POINT('',(-0.0577350269189626,-0.2,0.1));
#6618=CARTESIAN_POINT('Origin',(0.115470053837925,0.,0.));
#6619=CARTESIAN_POINT('',(0.122286297108185,0.,-0.0118060796608386));
#6620=CARTESIAN_POINT('',(0.0577350269189626,-0.2,0.1));
#6621=CARTESIAN_POINT('Origin',(0.,-0.2,0.));
#6622=CARTESIAN_POINT('Origin',(0.17,0.,0.));
#6623=CARTESIAN_POINT('',(-0.17,-8.67361737988404E-18,-2.0818995585505E-17));
#6624=CARTESIAN_POINT('Origin',(0.,0.,0.));
#6625=CARTESIAN_POINT('Origin',(0.,-0.015,0.));
#6626=CARTESIAN_POINT('',(-0.1954,-0.0254,-2.39295984553393E-17));
#6627=CARTESIAN_POINT('Origin',(0.,-0.0254,0.));
#6628=CARTESIAN_POINT('',(-0.185,-0.015,-2.2655965784226E-17));
#6629=CARTESIAN_POINT('Origin',(0.,-0.2775,0.));
#6630=CARTESIAN_POINT('',(-0.1954,-0.2775,-2.39295984553393E-17));
#6631=CARTESIAN_POINT('',(0.,0.,0.));
#6632=CARTESIAN_POINT('',(2.,3.46410161513775,5.25));
#6633=CARTESIAN_POINT('',(2.,3.46410161513775,2.75));
#6634=CARTESIAN_POINT('',(3.23743686707646,4.70153848221421,6.75));
#6635=CARTESIAN_POINT('',(0.762563132923542,4.70153848221421,6.75));
#6636=CARTESIAN_POINT('',(0.762563132923542,2.2266647480613,6.75));
#6637=CARTESIAN_POINT('',(3.23743686707646,2.2266647480613,6.75));
#6638=CARTESIAN_POINT('',(0.,0.,0.));
#6639=CARTESIAN_POINT('',(0.,0.,0.));
#6640=CARTESIAN_POINT('',(0.9,0.,1.4));
#6641=CARTESIAN_POINT('',(8.,0.,0.));
#6642=CARTESIAN_POINT('',(10.,3.46410161513775,5.25));
#6643=CARTESIAN_POINT('',(10.,3.46410161513775,2.75));
#6644=CARTESIAN_POINT('',(11.2374368670765,4.70153848221421,6.75));
#6645=CARTESIAN_POINT('',(8.76256313292354,4.70153848221421,6.75));
#6646=CARTESIAN_POINT('',(8.76256313292354,2.2266647480613,6.75));
#6647=CARTESIAN_POINT('',(11.2374368670765,2.2266647480613,6.75));
#6648=CARTESIAN_POINT('',(8.,0.,0.));
#6649=CARTESIAN_POINT('',(8.,0.,0.));
#6650=CARTESIAN_POINT('',(8.9,0.,1.4));
#6651=CARTESIAN_POINT('',(0.,0.,0.));
#6652=CARTESIAN_POINT('',(2.,3.46410161513775,2.75));
#6653=CARTESIAN_POINT('',(2.,3.46410161513775,2.75));
#6654=CARTESIAN_POINT('',(2.9,3.46410161513775,4.15));
#6655=CARTESIAN_POINT('',(10.,3.46410161513775,2.75));
#6656=CARTESIAN_POINT('',(10.,3.46410161513775,2.75));
#6657=CARTESIAN_POINT('',(10.9,3.46410161513775,4.15));
#6658=CARTESIAN_POINT('',(0.,0.,0.));
#6659=CARTESIAN_POINT('',(-3.06191609120998E-16,1.70926282564367E-32,-1.48769885299771E-14));
#6660=CARTESIAN_POINT('',(15.2523055207015,3.37699046999001,-8.73348857156638E-15));
#6661=CARTESIAN_POINT('',(-0.920784783198462,2.22470362076169,-1.71789432847248E-14));
#6662=UNCERTAINTY_MEASURE_WITH_UNIT(LENGTH_MEASURE(0.001),#6706,
'DISTANCE_ACCURACY_VALUE',
'Maximum model space distance between geometric entities at asserted c
onnectivities');
#6663=UNCERTAINTY_MEASURE_WITH_UNIT(LENGTH_MEASURE(0.001),#6706,
'DISTANCE_ACCURACY_VALUE',
'Maximum model space distance between geometric entities at asserted c
onnectivities');
#6664=UNCERTAINTY_MEASURE_WITH_UNIT(LENGTH_MEASURE(0.001),#6706,
'DISTANCE_ACCURACY_VALUE',
'Maximum model space distance between geometric entities at asserted c
onnectivities');
#6665=UNCERTAINTY_MEASURE_WITH_UNIT(LENGTH_MEASURE(0.001),#6706,
'DISTANCE_ACCURACY_VALUE',
'Maximum model space distance between geometric entities at asserted c
onnectivities');
#6666=UNCERTAINTY_MEASURE_WITH_UNIT(LENGTH_MEASURE(0.001),#6706,
'DISTANCE_ACCURACY_VALUE',
'Maximum model space distance between geometric entities at asserted c
onnectivities');
#6667=UNCERTAINTY_MEASURE_WITH_UNIT(LENGTH_MEASURE(0.001),#6706,
'DISTANCE_ACCURACY_VALUE',
'Maximum model space distance between geometric entities at asserted c
onnectivities');
#6668=UNCERTAINTY_MEASURE_WITH_UNIT(LENGTH_MEASURE(0.001),#6706,
'DISTANCE_ACCURACY_VALUE',
'Maximum model space distance between geometric entities at asserted c
onnectivities');
#6669=UNCERTAINTY_MEASURE_WITH_UNIT(LENGTH_MEASURE(0.001),#6706,
'DISTANCE_ACCURACY_VALUE',
'Maximum model space distance between geometric entities at asserted c
onnectivities');
#6670=UNCERTAINTY_MEASURE_WITH_UNIT(LENGTH_MEASURE(0.001),#6706,
'DISTANCE_ACCURACY_VALUE',
'Maximum model space distance between geometric entities at asserted c
onnectivities');
#6671=UNCERTAINTY_MEASURE_WITH_UNIT(LENGTH_MEASURE(0.001),#6706,
'DISTANCE_ACCURACY_VALUE',
'Maximum model space distance between geometric entities at asserted c
onnectivities');
#6672=UNCERTAINTY_MEASURE_WITH_UNIT(LENGTH_MEASURE(0.001),#6706,
'DISTANCE_ACCURACY_VALUE',
'Maximum model space distance between geometric entities at asserted c
onnectivities');
#6673=UNCERTAINTY_MEASURE_WITH_UNIT(LENGTH_MEASURE(0.001),#6706,
'DISTANCE_ACCURACY_VALUE',
'Maximum model space distance between geometric entities at asserted c
onnectivities');
#6674=UNCERTAINTY_MEASURE_WITH_UNIT(LENGTH_MEASURE(0.001),#6706,
'DISTANCE_ACCURACY_VALUE',
'Maximum model space distance between geometric entities at asserted c
onnectivities');
#6675=UNCERTAINTY_MEASURE_WITH_UNIT(LENGTH_MEASURE(0.001),#6706,
'DISTANCE_ACCURACY_VALUE',
'Maximum model space distance between geometric entities at asserted c
onnectivities');
#6676=UNCERTAINTY_MEASURE_WITH_UNIT(LENGTH_MEASURE(0.001),#6706,
'DISTANCE_ACCURACY_VALUE',
'Maximum model space distance between geometric entities at asserted c
onnectivities');
#6677=UNCERTAINTY_MEASURE_WITH_UNIT(LENGTH_MEASURE(0.001),#6706,
'DISTANCE_ACCURACY_VALUE',
'Maximum model space distance between geometric entities at asserted c
onnectivities');
#6678=UNCERTAINTY_MEASURE_WITH_UNIT(LENGTH_MEASURE(0.001),#6706,
'DISTANCE_ACCURACY_VALUE',
'Maximum model space distance between geometric entities at asserted c
onnectivities');
#6679=UNCERTAINTY_MEASURE_WITH_UNIT(LENGTH_MEASURE(0.001),#6706,
'DISTANCE_ACCURACY_VALUE',
'Maximum model space distance between geometric entities at asserted c
onnectivities');
#6680=UNCERTAINTY_MEASURE_WITH_UNIT(LENGTH_MEASURE(0.001),#6706,
'DISTANCE_ACCURACY_VALUE',
'Maximum model space distance between geometric entities at asserted c
onnectivities');
#6681=UNCERTAINTY_MEASURE_WITH_UNIT(LENGTH_MEASURE(0.001),#6706,
'DISTANCE_ACCURACY_VALUE',
'Maximum model space distance between geometric entities at asserted c
onnectivities');
#6682=UNCERTAINTY_MEASURE_WITH_UNIT(LENGTH_MEASURE(0.001),#6706,
'DISTANCE_ACCURACY_VALUE',
'Maximum model space distance between geometric entities at asserted c
onnectivities');
#6683=UNCERTAINTY_MEASURE_WITH_UNIT(LENGTH_MEASURE(0.001),#6706,
'DISTANCE_ACCURACY_VALUE',
'Maximum model space distance between geometric entities at asserted c
onnectivities');
#6684=(
GEOMETRIC_REPRESENTATION_CONTEXT(3)
GLOBAL_UNCERTAINTY_ASSIGNED_CONTEXT((#6662))
GLOBAL_UNIT_ASSIGNED_CONTEXT((#6706,#6708,#6709))
REPRESENTATION_CONTEXT('','3D')
);
#6685=(
GEOMETRIC_REPRESENTATION_CONTEXT(3)
GLOBAL_UNCERTAINTY_ASSIGNED_CONTEXT((#6663))
GLOBAL_UNIT_ASSIGNED_CONTEXT((#6706,#6708,#6709))
REPRESENTATION_CONTEXT('','3D')
);
#6686=(
GEOMETRIC_REPRESENTATION_CONTEXT(3)
GLOBAL_UNCERTAINTY_ASSIGNED_CONTEXT((#6664))
GLOBAL_UNIT_ASSIGNED_CONTEXT((#6706,#6708,#6709))
REPRESENTATION_CONTEXT('','3D')
);
#6687=(
GEOMETRIC_REPRESENTATION_CONTEXT(3)
GLOBAL_UNCERTAINTY_ASSIGNED_CONTEXT((#6665))
GLOBAL_UNIT_ASSIGNED_CONTEXT((#6706,#6708,#6709))
REPRESENTATION_CONTEXT('','3D')
);
#6688=(
GEOMETRIC_REPRESENTATION_CONTEXT(3)
GLOBAL_UNCERTAINTY_ASSIGNED_CONTEXT((#6666))
GLOBAL_UNIT_ASSIGNED_CONTEXT((#6706,#6708,#6709))
REPRESENTATION_CONTEXT('','3D')
);
#6689=(
GEOMETRIC_REPRESENTATION_CONTEXT(3)
GLOBAL_UNCERTAINTY_ASSIGNED_CONTEXT((#6667))
GLOBAL_UNIT_ASSIGNED_CONTEXT((#6706,#6708,#6709))
REPRESENTATION_CONTEXT('','3D')
);
#6690=(
GEOMETRIC_REPRESENTATION_CONTEXT(3)
GLOBAL_UNCERTAINTY_ASSIGNED_CONTEXT((#6668))
GLOBAL_UNIT_ASSIGNED_CONTEXT((#6706,#6708,#6709))
REPRESENTATION_CONTEXT('','3D')
);
#6691=(
GEOMETRIC_REPRESENTATION_CONTEXT(3)
GLOBAL_UNCERTAINTY_ASSIGNED_CONTEXT((#6669))
GLOBAL_UNIT_ASSIGNED_CONTEXT((#6706,#6708,#6709))
REPRESENTATION_CONTEXT('','3D')
);
#6692=(
GEOMETRIC_REPRESENTATION_CONTEXT(3)
GLOBAL_UNCERTAINTY_ASSIGNED_CONTEXT((#6670))
GLOBAL_UNIT_ASSIGNED_CONTEXT((#6706,#6708,#6709))
REPRESENTATION_CONTEXT('','3D')
);
#6693=(
GEOMETRIC_REPRESENTATION_CONTEXT(3)
GLOBAL_UNCERTAINTY_ASSIGNED_CONTEXT((#6671))
GLOBAL_UNIT_ASSIGNED_CONTEXT((#6706,#6708,#6709))
REPRESENTATION_CONTEXT('','3D')
);
#6694=(
GEOMETRIC_REPRESENTATION_CONTEXT(3)
GLOBAL_UNCERTAINTY_ASSIGNED_CONTEXT((#6672))
GLOBAL_UNIT_ASSIGNED_CONTEXT((#6706,#6708,#6709))
REPRESENTATION_CONTEXT('','3D')
);
#6695=(
GEOMETRIC_REPRESENTATION_CONTEXT(3)
GLOBAL_UNCERTAINTY_ASSIGNED_CONTEXT((#6673))
GLOBAL_UNIT_ASSIGNED_CONTEXT((#6706,#6708,#6709))
REPRESENTATION_CONTEXT('','3D')
);
#6696=(
GEOMETRIC_REPRESENTATION_CONTEXT(3)
GLOBAL_UNCERTAINTY_ASSIGNED_CONTEXT((#6674))
GLOBAL_UNIT_ASSIGNED_CONTEXT((#6706,#6708,#6709))
REPRESENTATION_CONTEXT('','3D')
);
#6697=(
GEOMETRIC_REPRESENTATION_CONTEXT(3)
GLOBAL_UNCERTAINTY_ASSIGNED_CONTEXT((#6675))
GLOBAL_UNIT_ASSIGNED_CONTEXT((#6706,#6708,#6709))
REPRESENTATION_CONTEXT('','3D')
);
#6698=(
GEOMETRIC_REPRESENTATION_CONTEXT(3)
GLOBAL_UNCERTAINTY_ASSIGNED_CONTEXT((#6676))
GLOBAL_UNIT_ASSIGNED_CONTEXT((#6706,#6708,#6709))
REPRESENTATION_CONTEXT('','3D')
);
#6699=(
GEOMETRIC_REPRESENTATION_CONTEXT(3)
GLOBAL_UNCERTAINTY_ASSIGNED_CONTEXT((#6677))
GLOBAL_UNIT_ASSIGNED_CONTEXT((#6706,#6708,#6709))
REPRESENTATION_CONTEXT('','3D')
);
#6700=(
GEOMETRIC_REPRESENTATION_CONTEXT(3)
GLOBAL_UNCERTAINTY_ASSIGNED_CONTEXT((#6678))
GLOBAL_UNIT_ASSIGNED_CONTEXT((#6706,#6708,#6709))
REPRESENTATION_CONTEXT('','3D')
);
#6701=(
GEOMETRIC_REPRESENTATION_CONTEXT(3)
GLOBAL_UNCERTAINTY_ASSIGNED_CONTEXT((#6679))
GLOBAL_UNIT_ASSIGNED_CONTEXT((#6706,#6708,#6709))
REPRESENTATION_CONTEXT('','3D')
);
#6702=(
GEOMETRIC_REPRESENTATION_CONTEXT(3)
GLOBAL_UNCERTAINTY_ASSIGNED_CONTEXT((#6680))
GLOBAL_UNIT_ASSIGNED_CONTEXT((#6706,#6708,#6709))
REPRESENTATION_CONTEXT('','3D')
);
#6703=(
GEOMETRIC_REPRESENTATION_CONTEXT(3)
GLOBAL_UNCERTAINTY_ASSIGNED_CONTEXT((#6681))
GLOBAL_UNIT_ASSIGNED_CONTEXT((#6706,#6708,#6709))
REPRESENTATION_CONTEXT('','3D')
);
#6704=(
GEOMETRIC_REPRESENTATION_CONTEXT(3)
GLOBAL_UNCERTAINTY_ASSIGNED_CONTEXT((#6682))
GLOBAL_UNIT_ASSIGNED_CONTEXT((#6706,#6708,#6709))
REPRESENTATION_CONTEXT('','3D')
);
#6705=(
GEOMETRIC_REPRESENTATION_CONTEXT(3)
GLOBAL_UNCERTAINTY_ASSIGNED_CONTEXT((#6683))
GLOBAL_UNIT_ASSIGNED_CONTEXT((#6706,#6708,#6709))
REPRESENTATION_CONTEXT('','3D')
);
#6706=(
LENGTH_UNIT()
NAMED_UNIT(*)
SI_UNIT(.CENTI.,.METRE.)
);
#6707=(
LENGTH_UNIT()
NAMED_UNIT(*)
SI_UNIT($,.METRE.)
);
#6708=(
NAMED_UNIT(*)
PLANE_ANGLE_UNIT()
SI_UNIT($,.RADIAN.)
);
#6709=(
NAMED_UNIT(*)
SI_UNIT($,.STERADIAN.)
SOLID_ANGLE_UNIT()
);
#6710=SHAPE_DEFINITION_REPRESENTATION(#6731,#6811);
#6711=SHAPE_DEFINITION_REPRESENTATION(#6732,#6812);
#6712=SHAPE_DEFINITION_REPRESENTATION(#6733,#6813);
#6713=SHAPE_DEFINITION_REPRESENTATION(#6734,#6814);
#6714=SHAPE_DEFINITION_REPRESENTATION(#6735,#6815);
#6715=SHAPE_DEFINITION_REPRESENTATION(#6736,#6816);
#6716=SHAPE_DEFINITION_REPRESENTATION(#6737,#6817);
#6717=SHAPE_DEFINITION_REPRESENTATION(#6738,#6818);
#6718=SHAPE_DEFINITION_REPRESENTATION(#6739,#6819);
#6719=SHAPE_DEFINITION_REPRESENTATION(#6740,#6820);
#6720=SHAPE_DEFINITION_REPRESENTATION(#6741,#6821);
#6721=SHAPE_DEFINITION_REPRESENTATION(#6742,#6822);
#6722=SHAPE_DEFINITION_REPRESENTATION(#6743,#6823);
#6723=SHAPE_DEFINITION_REPRESENTATION(#6744,#6824);
#6724=SHAPE_DEFINITION_REPRESENTATION(#6750,#6825);
#6725=SHAPE_DEFINITION_REPRESENTATION(#6751,#6826);
#6726=SHAPE_DEFINITION_REPRESENTATION(#6775,#6827);
#6727=SHAPE_DEFINITION_REPRESENTATION(#6776,#6828);
#6728=SHAPE_DEFINITION_REPRESENTATION(#6777,#6829);
#6729=SHAPE_DEFINITION_REPRESENTATION(#6778,#6830);
#6730=SHAPE_DEFINITION_REPRESENTATION(#6779,#6831);
#6731=PRODUCT_DEFINITION_SHAPE('',$,#6833);
#6732=PRODUCT_DEFINITION_SHAPE('',$,#6834);
#6733=PRODUCT_DEFINITION_SHAPE('',$,#6835);
#6734=PRODUCT_DEFINITION_SHAPE('',$,#6836);
#6735=PRODUCT_DEFINITION_SHAPE('',$,#6837);
#6736=PRODUCT_DEFINITION_SHAPE('',$,#6838);
#6737=PRODUCT_DEFINITION_SHAPE('',$,#6839);
#6738=PRODUCT_DEFINITION_SHAPE('',$,#6840);
#6739=PRODUCT_DEFINITION_SHAPE('',$,#6841);
#6740=PRODUCT_DEFINITION_SHAPE('',$,#6842);
#6741=PRODUCT_DEFINITION_SHAPE('',$,#6843);
#6742=PRODUCT_DEFINITION_SHAPE('',$,#6844);
#6743=PRODUCT_DEFINITION_SHAPE('',$,#6845);
#6744=PRODUCT_DEFINITION_SHAPE('',$,#6846);
#6745=PRODUCT_DEFINITION_SHAPE($,$,#188);
#6746=PRODUCT_DEFINITION_SHAPE($,$,#189);
#6747=PRODUCT_DEFINITION_SHAPE($,$,#190);
#6748=PRODUCT_DEFINITION_SHAPE($,$,#191);
#6749=PRODUCT_DEFINITION_SHAPE($,$,#192);
#6750=PRODUCT_DEFINITION_SHAPE('',$,#6847);
#6751=PRODUCT_DEFINITION_SHAPE('',$,#6848);
#6752=PRODUCT_DEFINITION_SHAPE($,$,#193);
#6753=PRODUCT_DEFINITION_SHAPE($,$,#194);
#6754=PRODUCT_DEFINITION_SHAPE($,$,#195);
#6755=PRODUCT_DEFINITION_SHAPE($,$,#196);
#6756=PRODUCT_DEFINITION_SHAPE($,$,#197);
#6757=PRODUCT_DEFINITION_SHAPE($,$,#198);
#6758=PRODUCT_DEFINITION_SHAPE($,$,#199);
#6759=PRODUCT_DEFINITION_SHAPE($,$,#200);
#6760=PRODUCT_DEFINITION_SHAPE($,$,#201);
#6761=PRODUCT_DEFINITION_SHAPE($,$,#202);
#6762=PRODUCT_DEFINITION_SHAPE($,$,#203);
#6763=PRODUCT_DEFINITION_SHAPE($,$,#204);
#6764=PRODUCT_DEFINITION_SHAPE($,$,#205);
#6765=PRODUCT_DEFINITION_SHAPE($,$,#206);
#6766=PRODUCT_DEFINITION_SHAPE($,$,#207);
#6767=PRODUCT_DEFINITION_SHAPE($,$,#208);
#6768=PRODUCT_DEFINITION_SHAPE($,$,#209);
#6769=PRODUCT_DEFINITION_SHAPE($,$,#210);
#6770=PRODUCT_DEFINITION_SHAPE($,$,#211);
#6771=PRODUCT_DEFINITION_SHAPE($,$,#212);
#6772=PRODUCT_DEFINITION_SHAPE($,$,#213);
#6773=PRODUCT_DEFINITION_SHAPE($,$,#214);
#6774=PRODUCT_DEFINITION_SHAPE($,$,#215);
#6775=PRODUCT_DEFINITION_SHAPE('',$,#6849);
#6776=PRODUCT_DEFINITION_SHAPE('',$,#6850);
#6777=PRODUCT_DEFINITION_SHAPE('',$,#6851);
#6778=PRODUCT_DEFINITION_SHAPE('',$,#6852);
#6779=PRODUCT_DEFINITION_SHAPE('',$,#6853);
#6780=PRODUCT_DEFINITION_SHAPE($,$,#216);
#6781=PRODUCT_DEFINITION_SHAPE($,$,#217);
#6782=PRODUCT_DEFINITION_SHAPE($,$,#218);
#6783=PRODUCT_DEFINITION_SHAPE($,$,#219);
#6784=PRODUCT_DEFINITION_SHAPE($,$,#220);
#6785=PRODUCT_DEFINITION_SHAPE($,$,#221);
#6786=PRODUCT_DEFINITION_SHAPE($,$,#222);
#6787=PRODUCT_DEFINITION_SHAPE($,$,#223);
#6788=PRODUCT_DEFINITION_SHAPE($,$,#224);
#6789=PRODUCT_DEFINITION_SHAPE($,$,#225);
#6790=PRODUCT_DEFINITION_SHAPE($,$,#226);
#6791=PRODUCT_DEFINITION_SHAPE($,$,#227);
#6792=PRODUCT_DEFINITION_SHAPE($,$,#228);
#6793=PRODUCT_DEFINITION_SHAPE($,$,#229);
#6794=PRODUCT_DEFINITION_SHAPE($,$,#230);
#6795=PRODUCT_DEFINITION_SHAPE($,$,#231);
#6796=PRODUCT_DEFINITION_SHAPE($,$,#232);
#6797=PRODUCT_DEFINITION_SHAPE($,$,#233);
#6798=PRODUCT_DEFINITION_SHAPE($,$,#234);
#6799=PRODUCT_DEFINITION_SHAPE($,$,#235);
#6800=PRODUCT_DEFINITION_SHAPE($,$,#236);
#6801=PRODUCT_DEFINITION_SHAPE($,$,#237);
#6802=PRODUCT_DEFINITION_SHAPE($,$,#238);
#6803=PRODUCT_DEFINITION_SHAPE($,$,#239);
#6804=PRODUCT_DEFINITION_SHAPE($,$,#240);
#6805=PRODUCT_DEFINITION_SHAPE($,$,#241);
#6806=PRODUCT_DEFINITION_SHAPE($,$,#242);
#6807=PRODUCT_DEFINITION_SHAPE($,$,#243);
#6808=PRODUCT_DEFINITION_SHAPE($,$,#244);
#6809=PRODUCT_DEFINITION_SHAPE($,$,#245);
#6810=PRODUCT_DEFINITION_SHAPE($,$,#246);
#6811=SHAPE_REPRESENTATION('',(#3572,#4062,#4063,#4064,#4065),#6684);
#6812=SHAPE_REPRESENTATION('',(#3573,#3946,#3947,#3948,#3949,#3950,#3951,
#3952,#3953,#3954,#3955,#3956,#3957,#3958,#3959,#3960,#3961,#3962,#3963,
#3964,#3965,#3966,#3967,#3968),#6685);
#6813=SHAPE_REPRESENTATION('',(#3574),#6686);
#6814=SHAPE_REPRESENTATION('',(#3605),#6687);
#6815=SHAPE_REPRESENTATION('',(#3675),#6688);
#6816=SHAPE_REPRESENTATION('',(#3699,#4035,#4036,#4037,#4038,#4039,#4040,
#4041,#4042,#4043,#4044),#6689);
#6817=SHAPE_REPRESENTATION('',(#3700,#4045,#4046,#4047,#4048,#4049,#4050,
#4051,#4052,#4053,#4054),#6690);
#6818=SHAPE_REPRESENTATION('',(#3701),#6691);
#6819=SHAPE_REPRESENTATION('',(#3747,#3876,#3877,#3878,#3879,#3880),#6692);
#6820=SHAPE_REPRESENTATION('',(#3748),#6693);
#6821=SHAPE_REPRESENTATION('',(#3768),#6694);
#6822=SHAPE_REPRESENTATION('',(#3788),#6695);
#6823=SHAPE_REPRESENTATION('',(#3805),#6696);
#6824=SHAPE_REPRESENTATION('',(#3859),#6697);
#6825=SHAPE_REPRESENTATION('',(#3881),#6698);
#6826=SHAPE_REPRESENTATION('',(#3922),#6699);
#6827=SHAPE_REPRESENTATION('',(#3969,#4055,#4056,#4057,#4058,#4059,#4060,
#4061),#6700);
#6828=SHAPE_REPRESENTATION('',(#3970),#6701);
#6829=SHAPE_REPRESENTATION('',(#3997),#6702);
#6830=SHAPE_REPRESENTATION('',(#4006),#6703);
#6831=SHAPE_REPRESENTATION('',(#4020),#6704);
#6832=PRODUCT_DEFINITION_CONTEXT('part definition',#6897,'design');
#6833=PRODUCT_DEFINITION('PAT-040',
'PAT-040',#6854,#6832);
#6834=PRODUCT_DEFINITION('Base and fixed pivots',
'Base and fixed pivots',#6855,#6832);
#6835=PRODUCT_DEFINITION('Tabletop base','Tabletop base',#6856,#6832);
#6836=PRODUCT_DEFINITION('Pivot pedestal','Pivot pedestal',#6857,#6832);
#6837=PRODUCT_DEFINITION('M5x14 Cap Screw','M5x14 Cap Screw',#6858,#6832);
#6838=PRODUCT_DEFINITION('First crank','First crank',#6859,#6832);
#6839=PRODUCT_DEFINITION('Second crank','Second crank',#6860,#6832);
#6840=PRODUCT_DEFINITION('Forty millimetre crank',
'Forty millimetre crank',#6861,#6832);
#6841=PRODUCT_DEFINITION('Sealed Ball Bearing - 10 x 30 x 9 mm',
'Sealed Ball Bearing - 10 x 30 x 9 mm',#6862,#6832);
#6842=PRODUCT_DEFINITION('Inner ring','Inner ring',#6863,#6832);
#6843=PRODUCT_DEFINITION('Outer ring','Outer ring',#6864,#6832);
#6844=PRODUCT_DEFINITION('Balls','Balls',#6865,#6832);
#6845=PRODUCT_DEFINITION('Cage','Cage',#6866,#6832);
#6846=PRODUCT_DEFINITION('Seals 2RS','Seals 2RS',#6867,#6832);
#6847=PRODUCT_DEFINITION('Pivot cap','Pivot cap',#6868,#6832);
#6848=PRODUCT_DEFINITION('M4x10 Cap Screw','M4x10 Cap Screw',#6869,#6832);
#6849=PRODUCT_DEFINITION('Parallel coupler','Parallel coupler',#6870,#6832);
#6850=PRODUCT_DEFINITION('Eighty millimetre coupler and pins',
'Eighty millimetre coupler and pins',#6871,#6832);
#6851=PRODUCT_DEFINITION('Lower race sleeve','Lower race sleeve',#6872,
#6832);
#6852=PRODUCT_DEFINITION('Spindle collar','Spindle collar',#6873,#6832);
#6853=PRODUCT_DEFINITION('M4x4 collar screw','M4x4 collar screw',#6874,
#6832);
#6854=PRODUCT_DEFINITION_FORMATION('',$,#6899);
#6855=PRODUCT_DEFINITION_FORMATION('',$,#6900);
#6856=PRODUCT_DEFINITION_FORMATION('',$,#6901);
#6857=PRODUCT_DEFINITION_FORMATION('',$,#6902);
#6858=PRODUCT_DEFINITION_FORMATION('',$,#6903);
#6859=PRODUCT_DEFINITION_FORMATION('',$,#6904);
#6860=PRODUCT_DEFINITION_FORMATION('',$,#6905);
#6861=PRODUCT_DEFINITION_FORMATION('',$,#6906);
#6862=PRODUCT_DEFINITION_FORMATION('',$,#6907);
#6863=PRODUCT_DEFINITION_FORMATION('',$,#6908);
#6864=PRODUCT_DEFINITION_FORMATION('',$,#6909);
#6865=PRODUCT_DEFINITION_FORMATION('',$,#6910);
#6866=PRODUCT_DEFINITION_FORMATION('',$,#6911);
#6867=PRODUCT_DEFINITION_FORMATION('',$,#6912);
#6868=PRODUCT_DEFINITION_FORMATION('',$,#6913);
#6869=PRODUCT_DEFINITION_FORMATION('',$,#6914);
#6870=PRODUCT_DEFINITION_FORMATION('',$,#6915);
#6871=PRODUCT_DEFINITION_FORMATION('',$,#6916);
#6872=PRODUCT_DEFINITION_FORMATION('',$,#6917);
#6873=PRODUCT_DEFINITION_FORMATION('',$,#6918);
#6874=PRODUCT_DEFINITION_FORMATION('',$,#6919);
#6875=PRODUCT_RELATED_PRODUCT_CATEGORY('PAT-040',
'PAT-040',(#6899));
#6876=PRODUCT_RELATED_PRODUCT_CATEGORY('Base and fixed pivots',
'Base and fixed pivots',(#6900));
#6877=PRODUCT_RELATED_PRODUCT_CATEGORY('Tabletop base','Tabletop base',
(#6901));
#6878=PRODUCT_RELATED_PRODUCT_CATEGORY('Pivot pedestal',
'Pivot pedestal',(#6902));
#6879=PRODUCT_RELATED_PRODUCT_CATEGORY('M5x14 Cap Screw',
'M5x14 Cap Screw',(#6903));
#6880=PRODUCT_RELATED_PRODUCT_CATEGORY('First crank','First crank',(#6904));
#6881=PRODUCT_RELATED_PRODUCT_CATEGORY('Second crank','Second crank',(#6905));
#6882=PRODUCT_RELATED_PRODUCT_CATEGORY('Forty millimetre crank',
'Forty millimetre crank',(#6906));
#6883=PRODUCT_RELATED_PRODUCT_CATEGORY(
'Sealed Ball Bearing - 10 x 30 x 9 mm',
'Sealed Ball Bearing - 10 x 30 x 9 mm',(#6907));
#6884=PRODUCT_RELATED_PRODUCT_CATEGORY('Inner ring','Inner ring',(#6908));
#6885=PRODUCT_RELATED_PRODUCT_CATEGORY('Outer ring','Outer ring',(#6909));
#6886=PRODUCT_RELATED_PRODUCT_CATEGORY('Balls','Balls',(#6910));
#6887=PRODUCT_RELATED_PRODUCT_CATEGORY('Cage','Cage',(#6911));
#6888=PRODUCT_RELATED_PRODUCT_CATEGORY('Seals 2RS','Seals 2RS',(#6912));
#6889=PRODUCT_RELATED_PRODUCT_CATEGORY('Pivot cap','Pivot cap',(#6913));
#6890=PRODUCT_RELATED_PRODUCT_CATEGORY('M4x10 Cap Screw',
'M4x10 Cap Screw',(#6914));
#6891=PRODUCT_RELATED_PRODUCT_CATEGORY('Parallel coupler',
'Parallel coupler',(#6915));
#6892=PRODUCT_RELATED_PRODUCT_CATEGORY(
'Eighty millimetre coupler and pins',
'Eighty millimetre coupler and pins',(#6916));
#6893=PRODUCT_RELATED_PRODUCT_CATEGORY('Lower race sleeve',
'Lower race sleeve',(#6917));
#6894=PRODUCT_RELATED_PRODUCT_CATEGORY('Spindle collar',
'Spindle collar',(#6918));
#6895=PRODUCT_RELATED_PRODUCT_CATEGORY('M4x4 collar screw',
'M4x4 collar screw',(#6919));
#6896=APPLICATION_PROTOCOL_DEFINITION('international standard',
'automotive_design',2009,#6897);
#6897=APPLICATION_CONTEXT(
'Core Data for Automotive Mechanical Design Process');
#6898=PRODUCT_CONTEXT('part definition',#6897,'mechanical');
#6899=PRODUCT('PAT-040',
'PAT-040','PAT-040',(#6898));
#6900=PRODUCT('Base and fixed pivots','Base and fixed pivots',
'Base and fixed pivots',(#6898));
#6901=PRODUCT('Tabletop base','Tabletop base','Tabletop base',(#6898));
#6902=PRODUCT('Pivot pedestal','Pivot pedestal','Pivot pedestal',(#6898));
#6903=PRODUCT('M5x14 Cap Screw','M5x14 Cap Screw','M5x14 Cap Screw',(#6898));
#6904=PRODUCT('First crank','First crank','First crank',(#6898));
#6905=PRODUCT('Second crank','Second crank','Second crank',(#6898));
#6906=PRODUCT('Forty millimetre crank','Forty millimetre crank',
'Forty millimetre crank',(#6898));
#6907=PRODUCT('Sealed Ball Bearing - 10 x 30 x 9 mm',
'Sealed Ball Bearing - 10 x 30 x 9 mm',
'Sealed Ball Bearing - 10 x 30 x 9 mm',(#6898));
#6908=PRODUCT('Inner ring','Inner ring','Inner ring',(#6898));
#6909=PRODUCT('Outer ring','Outer ring','Outer ring',(#6898));
#6910=PRODUCT('Balls','Balls','Balls',(#6898));
#6911=PRODUCT('Cage','Cage','Cage',(#6898));
#6912=PRODUCT('Seals 2RS','Seals 2RS','Seals 2RS',(#6898));
#6913=PRODUCT('Pivot cap','Pivot cap','Pivot cap',(#6898));
#6914=PRODUCT('M4x10 Cap Screw','M4x10 Cap Screw','M4x10 Cap Screw',(#6898));
#6915=PRODUCT('Parallel coupler','Parallel coupler','Parallel coupler',
(#6898));
#6916=PRODUCT('Eighty millimetre coupler and pins',
'Eighty millimetre coupler and pins',
'Eighty millimetre coupler and pins',(#6898));
#6917=PRODUCT('Lower race sleeve','Lower race sleeve',
'Lower race sleeve',(#6898));
#6918=PRODUCT('Spindle collar','Spindle collar','Spindle collar',(#6898));
#6919=PRODUCT('M4x4 collar screw','M4x4 collar screw',
'M4x4 collar screw',(#6898));
#6920=PRESENTATION_STYLE_ASSIGNMENT((#6926));
#6921=PRESENTATION_STYLE_ASSIGNMENT((#6927));
#6922=PRESENTATION_STYLE_ASSIGNMENT((#6928));
#6923=PRESENTATION_STYLE_ASSIGNMENT((#6929));
#6924=PRESENTATION_STYLE_ASSIGNMENT((#6930));
#6925=PRESENTATION_STYLE_ASSIGNMENT((#6931));
#6926=SURFACE_STYLE_USAGE(.BOTH.,#6932);
#6927=SURFACE_STYLE_USAGE(.BOTH.,#6933);
#6928=SURFACE_STYLE_USAGE(.BOTH.,#6934);
#6929=SURFACE_STYLE_USAGE(.BOTH.,#6935);
#6930=SURFACE_STYLE_USAGE(.BOTH.,#6936);
#6931=SURFACE_STYLE_USAGE(.BOTH.,#6937);
#6932=SURFACE_SIDE_STYLE('',(#6938));
#6933=SURFACE_SIDE_STYLE('',(#6939));
#6934=SURFACE_SIDE_STYLE('',(#6940));
#6935=SURFACE_SIDE_STYLE('',(#6941));
#6936=SURFACE_SIDE_STYLE('',(#6942));
#6937=SURFACE_SIDE_STYLE('',(#6943));
#6938=SURFACE_STYLE_FILL_AREA(#6944);
#6939=SURFACE_STYLE_FILL_AREA(#6945);
#6940=SURFACE_STYLE_FILL_AREA(#6946);
#6941=SURFACE_STYLE_FILL_AREA(#6947);
#6942=SURFACE_STYLE_FILL_AREA(#6948);
#6943=SURFACE_STYLE_FILL_AREA(#6949);
#6944=FILL_AREA_STYLE('Steel - Satin',(#6950));
#6945=FILL_AREA_STYLE('CAD Library Painted - Deep blue',(#6951));
#6946=FILL_AREA_STYLE('CAD Library Painted - Engineering blue',(#6952));
#6947=FILL_AREA_STYLE('CAD Library Painted - Graphite',(#6953));
#6948=FILL_AREA_STYLE('CAD Library Painted - Steel gray',(#6954));
#6949=FILL_AREA_STYLE('CAD Library Painted - Off white',(#6955));
#6950=FILL_AREA_STYLE_COLOUR('Steel - Satin',#6956);
#6951=FILL_AREA_STYLE_COLOUR('CAD Library Painted - Deep blue',#6957);
#6952=FILL_AREA_STYLE_COLOUR('CAD Library Painted - Engineering blue',#6958);
#6953=FILL_AREA_STYLE_COLOUR('CAD Library Painted - Graphite',#6959);
#6954=FILL_AREA_STYLE_COLOUR('CAD Library Painted - Steel gray',#6960);
#6955=FILL_AREA_STYLE_COLOUR('CAD Library Painted - Off white',#6961);
#6956=COLOUR_RGB('Steel - Satin',0.627450980392157,0.627450980392157,0.627450980392157);
#6957=COLOUR_RGB('CAD Library Painted - Deep blue',0.0784313725490196,0.203921568627451,
0.349019607843137);
#6958=COLOUR_RGB('CAD Library Painted - Engineering blue',0.12156862745098,
0.356862745098039,0.6);
#6959=COLOUR_RGB('CAD Library Painted - Graphite',0.0980392156862745,0.109803921568627,
0.125490196078431);
#6960=COLOUR_RGB('CAD Library Painted - Steel gray',0.592156862745098,0.631372549019608,
0.67843137254902);
#6961=COLOUR_RGB('CAD Library Painted - Off white',0.909803921568627,0.901960784313726,
0.858823529411765);
#6962=COLOUR_RGB('Dark Blue',0.08,0.2,0.34);
#6963=FILL_AREA_STYLE_COLOUR('',#6962);
#6964=FILL_AREA_STYLE('',(#6963));
#6965=SURFACE_STYLE_FILL_AREA(#6964);
#6966=SURFACE_SIDE_STYLE('',(#6965));
#6967=SURFACE_STYLE_USAGE(.BOTH.,#6966);
#6968=PRESENTATION_STYLE_ASSIGNMENT((#6967));
#6969=COLOUR_RGB('Light Blue',0.38,0.62,0.78);
#6970=FILL_AREA_STYLE_COLOUR('',#6969);
#6971=FILL_AREA_STYLE('',(#6970));
#6972=SURFACE_STYLE_FILL_AREA(#6971);
#6973=SURFACE_SIDE_STYLE('',(#6972));
#6974=SURFACE_STYLE_USAGE(.BOTH.,#6973);
#6975=PRESENTATION_STYLE_ASSIGNMENT((#6974));
#6976=COLOUR_RGB('Sky Blue',0.24,0.69,0.87);
#6977=FILL_AREA_STYLE_COLOUR('',#6976);
#6978=FILL_AREA_STYLE('',(#6977));
#6979=SURFACE_STYLE_FILL_AREA(#6978);
#6980=SURFACE_SIDE_STYLE('',(#6979));
#6981=SURFACE_STYLE_USAGE(.BOTH.,#6980);
#6982=PRESENTATION_STYLE_ASSIGNMENT((#6981));
#6983=COLOUR_RGB('Grey',0.48,0.52,0.57);
#6984=FILL_AREA_STYLE_COLOUR('',#6983);
#6985=FILL_AREA_STYLE('',(#6984));
#6986=SURFACE_STYLE_FILL_AREA(#6985);
#6987=SURFACE_SIDE_STYLE('',(#6986));
#6988=SURFACE_STYLE_USAGE(.BOTH.,#6987);
#6989=PRESENTATION_STYLE_ASSIGNMENT((#6988));
#6990=COLOUR_RGB('Black',0.12,0.14,0.17);
#6991=FILL_AREA_STYLE_COLOUR('',#6990);
#6992=FILL_AREA_STYLE('',(#6991));
#6993=SURFACE_STYLE_FILL_AREA(#6992);
#6994=SURFACE_SIDE_STYLE('',(#6993));
#6995=SURFACE_STYLE_USAGE(.BOTH.,#6994);
#6996=PRESENTATION_STYLE_ASSIGNMENT((#6995));
#6997=COLOUR_RGB('Off White',0.89,0.88,0.83);
#6998=FILL_AREA_STYLE_COLOUR('',#6997);
#6999=FILL_AREA_STYLE('',(#6998));
#7000=SURFACE_STYLE_FILL_AREA(#6999);
#7001=SURFACE_SIDE_STYLE('',(#7000));
#7002=SURFACE_STYLE_USAGE(.BOTH.,#7001);
#7003=PRESENTATION_STYLE_ASSIGNMENT((#7002));
ENDSEC;
END-ISO-10303-21;
